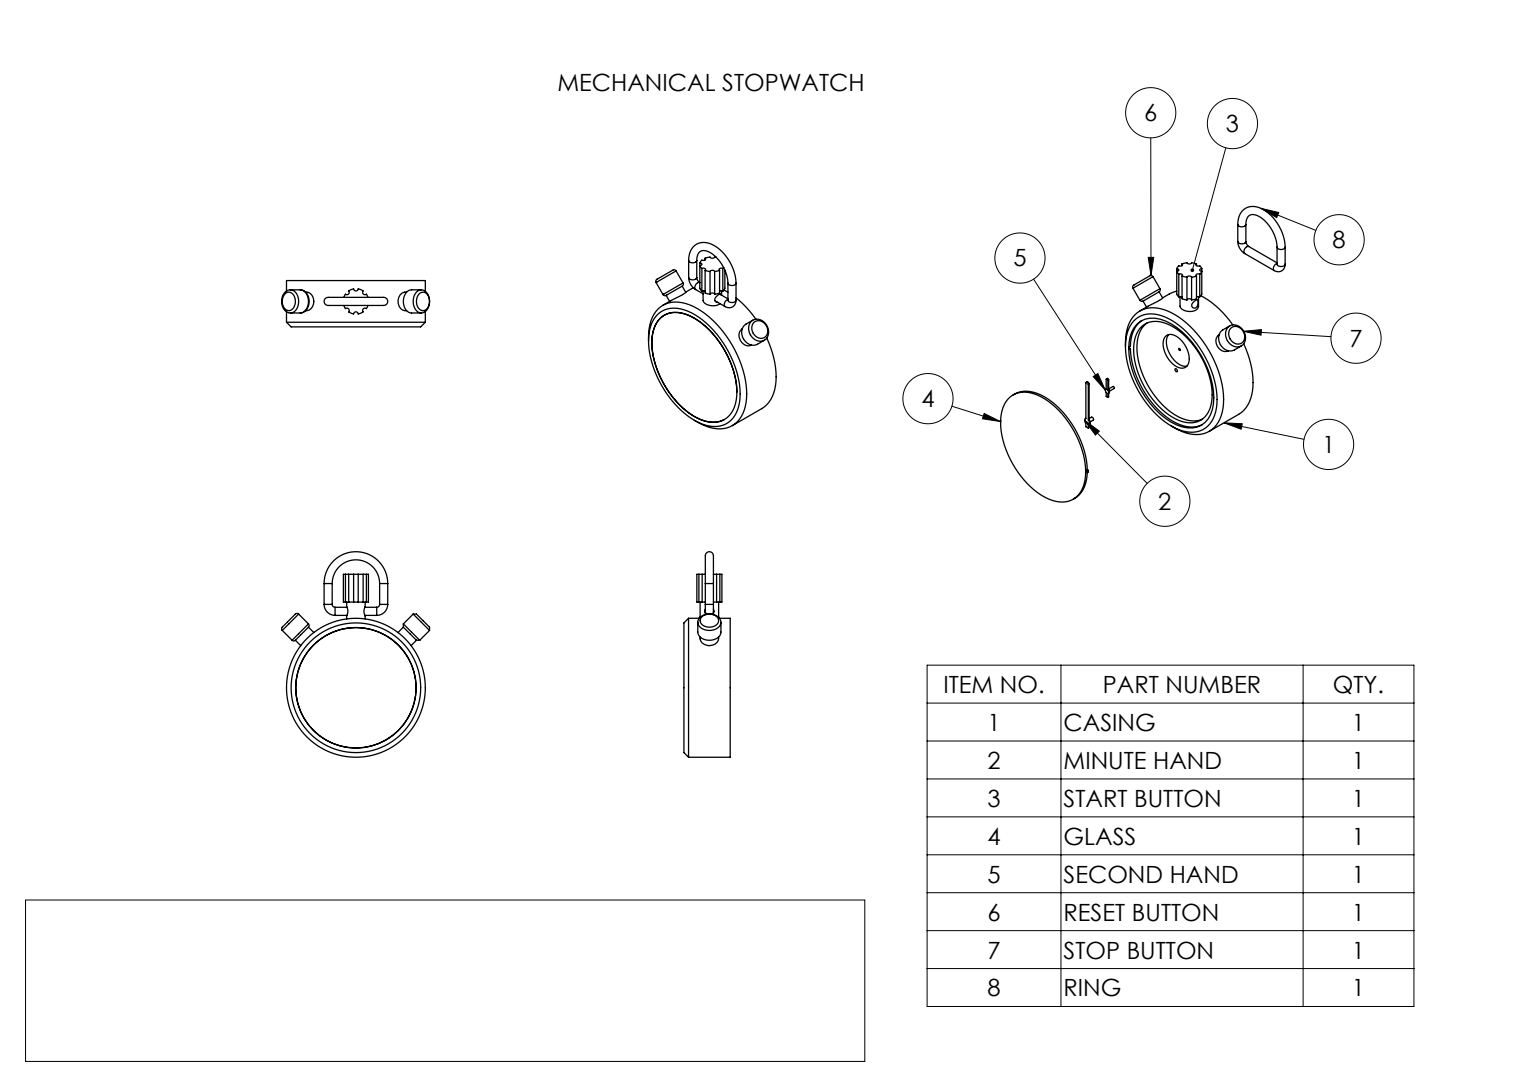
ISO-10303-21;
HEADER;
FILE_DESCRIPTION (('STEP AP214'),
    '1' );
FILE_NAME ('MAS-171',
    '2026-10-26T11:20:31',
    ( '' ),
    ( '' ),
    'SwSTEP 2.0',
    'SolidWorks 2026',
    '' );
FILE_SCHEMA (( 'AUTOMOTIVE_DESIGN' ));
ENDSEC;

DATA;
#1 = CARTESIAN_POINT ( 'NONE',  ( -0.7500000000000000000, 0.000000000000000000, 17.69999999999999929 ) ) ;
#2 = ORIENTED_EDGE ( 'NONE', *, *, #1110, .F. ) ;
#3 = ORIENTED_EDGE ( 'NONE', *, *, #2058, .T. ) ;
#4 = DIRECTION ( 'NONE',  ( 1.000000000000000000, 0.000000000000000000, 0.000000000000000000 ) ) ;
#5 = DIRECTION ( 'NONE',  ( 0.000000000000000000, 0.000000000000000000, 1.000000000000000000 ) ) ;
#6 = ORIENTED_EDGE ( 'NONE', *, *, #2251, .T. ) ;
#7 = ORIENTED_EDGE ( 'NONE', *, *, #1306, .T. ) ;
#8 = ORIENTED_EDGE ( 'NONE', *, *, #613, .T. ) ;
#9 = FACE_OUTER_BOUND ( 'NONE', #3478, .T. ) ;
#10 = MECHANICAL_DESIGN_GEOMETRIC_PRESENTATION_REPRESENTATION (  '', ( #2667 ), #1914 ) ;
#11 = CARTESIAN_POINT ( 'NONE',  ( 3.575465955037824273, 33.89312899261130951, 7.205771075917312807 ) ) ;
#12 = FILL_AREA_STYLE ('',( #728 ) ) ;
#13 = CARTESIAN_POINT ( 'NONE',  ( 3.900351855253538336, 31.20702153671021861, 9.895868398202676275 ) ) ;
#14 = APPLICATION_PROTOCOL_DEFINITION ( 'draft international standard', 'automotive_design', 1998, #590 ) ;
#15 = CIRCLE ( 'NONE', #3506, 24.00000000000000355 ) ;
#16 = AXIS2_PLACEMENT_3D ( 'NONE', #2193, #1531, #438 ) ;
#17 = CARTESIAN_POINT ( 'NONE',  ( 23.85222316637485562, 18.19536891688241198, 8.735393166554770161 ) ) ;
#18 = DIRECTION ( 'NONE',  ( -0.000000000000000000, -0.000000000000000000, -1.000000000000000000 ) ) ;
#19 = CARTESIAN_POINT ( 'NONE',  ( -0.5000000000000000000, -2.999999999999999556, 19.50000000000000000 ) ) ;
#20 = AXIS2_PLACEMENT_3D ( 'NONE', #4406, #1830, #790 ) ;
#21 = ORIENTED_EDGE ( 'NONE', *, *, #745, .T. ) ;
#22 = VERTEX_POINT ( 'NONE', #4223 ) ;
#23 = EDGE_CURVE ( 'NONE', #3682, #3477, #99, .T. ) ;
#24 = EDGE_CURVE ( 'NONE', #786, #1876, #1622, .T. ) ;
#25 = CARTESIAN_POINT ( 'NONE',  ( -3.889087296526001047, 37.00000000000000000, 5.110912703473974084 ) ) ;
#26 = DIRECTION ( 'NONE',  ( 0.000000000000000000, 0.000000000000000000, -1.000000000000000000 ) ) ;
#27 = VERTEX_POINT ( 'NONE', #607 ) ;
#28 = ORIENTED_EDGE ( 'NONE', *, *, #250, .F. ) ;
#29 = VERTEX_POINT ( 'NONE', #4130 ) ;
#30 = CARTESIAN_POINT ( 'NONE',  ( -8.999999999999998224, 36.00000000000000711, 0.000000000000000000 ) ) ;
#31 = CARTESIAN_POINT ( 'NONE',  ( -23.83674813237297130, 18.21571070649537916, 9.520895848189303123 ) ) ;
#32 =( LENGTH_UNIT ( ) NAMED_UNIT ( * ) SI_UNIT ( .MILLI., .METRE. ) );
#33 = CARTESIAN_POINT ( 'NONE',  ( -25.16843286583315376, -6.741346781237213648, 20.00001200000000168 ) ) ;
#34 = ORIENTED_EDGE ( 'NONE', *, *, #3765, .T. ) ;
#35 = APPLICATION_CONTEXT ( 'automotive_design' ) ;
#36 = AXIS2_PLACEMENT_3D ( 'NONE', #4466, #800, #1180 ) ;
#37 = CARTESIAN_POINT ( 'NONE',  ( 0.5000000000000001110, 6.123233995736767268E-17, 20.00000000000000000 ) ) ;
#38 = CARTESIAN_POINT ( 'NONE',  ( 0.000000000000000000, 10.00000000000000000, 13.00000000000000178 ) ) ;
#39 = CIRCLE ( 'NONE', #1106, 4.000000000000000000 ) ;
#40 = CARTESIAN_POINT ( 'NONE',  ( 18.61772044889877264, 23.52449179749628883, 6.992605352578564748 ) ) ;
#41 = CARTESIAN_POINT ( 'NONE',  ( -3.013274039476890653, 29.84885987243285399, 6.356496494711869616 ) ) ;
#42 = DIRECTION ( 'NONE',  ( 0.000000000000000000, 0.000000000000000000, 1.000000000000000000 ) ) ;
#43 = MECHANICAL_DESIGN_GEOMETRIC_PRESENTATION_REPRESENTATION (  '', ( #878 ), #2695 ) ;
#44 = ORIENTED_EDGE ( 'NONE', *, *, #3267, .F. ) ;
#45 = EDGE_CURVE ( 'NONE', #4134, #2111, #508, .T. ) ;
#46 = ORIENTED_EDGE ( 'NONE', *, *, #3772, .T. ) ;
#47 = CARTESIAN_POINT ( 'NONE',  ( -3.606497132222527213, 31.99144327829980838, 10.73188315364928691 ) ) ;
#48 = CIRCLE ( 'NONE', #1190, 1.749999999999999778 ) ;
#49 = DIRECTION ( 'NONE',  ( -0.000000000000000000, -0.000000000000000000, -1.000000000000000000 ) ) ;
#50 = EDGE_CURVE ( 'NONE', #1185, #1168, #2904, .T. ) ;
#51 = ORIENTED_EDGE ( 'NONE', *, *, #696, .F. ) ;
#52 = VERTEX_POINT ( 'NONE', #2322 ) ;
#53 = ORIENTED_EDGE ( 'NONE', *, *, #2142, .T. ) ;
#54 = EDGE_CURVE ( 'NONE', #3353, #742, #2591, .T. ) ;
#55 = CIRCLE ( 'NONE', #1867, 1.000000000000000000 ) ;
#56 = DIRECTION ( 'NONE',  ( 1.000000000000000000, 0.000000000000000000, -0.000000000000000000 ) ) ;
#57 = LINE ( 'NONE', #2588, #2669 ) ;
#58 = CARTESIAN_POINT ( 'NONE',  ( -0.5000000000000000000, 0.000000000000000000, 20.00000000000000000 ) ) ;
#59 = DIRECTION ( 'NONE',  ( 1.000000000000000000, 0.000000000000000000, 0.000000000000000000 ) ) ;
#60 = ORIENTED_EDGE ( 'NONE', *, *, #514, .T. ) ;
#61 = CARTESIAN_POINT ( 'NONE',  ( 3.120626071653185285, 37.00000000000000000, 4.471016347907789346 ) ) ;
#62 = DIRECTION ( 'NONE',  ( 0.000000000000000000, 0.000000000000000000, 1.000000000000000000 ) ) ;
#63 = CIRCLE ( 'NONE', #1740, 4.000000000000000000 ) ;
#64 = CARTESIAN_POINT ( 'NONE',  ( 21.58020450303990145, 20.84134157445924274, 5.025533726064748130 ) ) ;
#65 = DIRECTION ( 'NONE',  ( 0.000000000000000000, 1.000000000000000000, 0.000000000000000000 ) ) ;
#66 = TOROIDAL_SURFACE ( 'NONE', #1579, 12.00000000000000000, 1.749999999999999778 ) ;
#67 = FACE_OUTER_BOUND ( 'NONE', #3163, .T. ) ;
#68 = ADVANCED_FACE ( 'NONE', ( #4153 ), #1596, .T. ) ;
#69 = ORIENTED_EDGE ( 'NONE', *, *, #4531, .T. ) ;
#70 = ORIENTED_EDGE ( 'NONE', *, *, #687, .T. ) ;
#71 = EDGE_CURVE ( 'NONE', #1336, #2657, #200, .T. ) ;
#72 = AXIS2_PLACEMENT_3D ( 'NONE', #1710, #1001, #219 ) ;
#73 = CARTESIAN_POINT ( 'NONE',  ( -3.522877905629562711, 32.34829198493223146, 10.89542184998092367 ) ) ;
#74 = CARTESIAN_POINT ( 'NONE',  ( 3.469446951953614189E-15, 34.00000000000000000, 3.999999999999990674 ) ) ;
#75 = ORIENTED_EDGE ( 'NONE', *, *, #1897, .F. ) ;
#76 = EDGE_LOOP ( 'NONE', ( #1998, #356, #1571, #3856 ) ) ;
#77 = CIRCLE ( 'NONE', #3336, 1.749999999999999778 ) ;
#78 = ORIENTED_EDGE ( 'NONE', *, *, #3001, .F. ) ;
#79 = UNCERTAINTY_MEASURE_WITH_UNIT (LENGTH_MEASURE( 1.000000000000000082E-05 ), #706, 'distance_accuracy_value', 'NONE');
#80 = DIRECTION ( 'NONE',  ( 1.000000000000000000, -1.621111868633889227E-15, 0.000000000000000000 ) ) ;
#81 = CARTESIAN_POINT ( 'NONE',  ( -18.19536891688249014, 23.85222316637480233, 9.264542937126581279 ) ) ;
#82 = DIRECTION ( 'NONE',  ( 1.000000000000000000, 0.000000000000000000, 0.000000000000000000 ) ) ;
#83 = PLANE ( 'NONE',  #429 ) ;
#84 = EDGE_CURVE ( 'NONE', #2338, #1148, #4563, .T. ) ;
#85 = VERTEX_POINT ( 'NONE', #4577 ) ;
#86 = EDGE_CURVE ( 'NONE', #3119, #3855, #2573, .T. ) ;
#87 = LINE ( 'NONE', #2519, #444 ) ;
#88 = FACE_OUTER_BOUND ( 'NONE', #3234, .T. ) ;
#89 = CONTEXT_DEPENDENT_SHAPE_REPRESENTATION ( #4410, #2595 ) ;
#90 = AXIS2_PLACEMENT_3D ( 'NONE', #2223, #2270, #1567 ) ;
#91 = EDGE_CURVE ( 'NONE', #668, #4199, #3027, .T. ) ;
#92 = CARTESIAN_POINT ( 'NONE',  ( 23.23634976112698780, 18.97646788767667303, 6.355262957884884933 ) ) ;
#93 = PLANE ( 'NONE',  #36 ) ;
#94 = LINE ( 'NONE', #3342, #4161 ) ;
#95 = ORIENTED_EDGE ( 'NONE', *, *, #3675, .F. ) ;
#96 = ORIENTED_EDGE ( 'NONE', *, *, #3914, .F. ) ;
#97 = CARTESIAN_POINT ( 'NONE',  ( 0.000000000000000000, 0.000000000000000000, 17.69999999999999929 ) ) ;
#98 = DIRECTION ( 'NONE',  ( 0.000000000000000000, 0.000000000000000000, 1.000000000000000000 ) ) ;
#99 = CIRCLE ( 'NONE', #4660, 24.00000000000000355 ) ;
#100 = CIRCLE ( 'NONE', #1688, 1.749999999999999778 ) ;
#101 = CYLINDRICAL_SURFACE ( 'NONE', #1304, 4.000000000000000000 ) ;
#102 = VERTEX_POINT ( 'NONE', #652 ) ;
#103 = EDGE_LOOP ( 'NONE', ( #598, #2944, #3052, #880 ) ) ;
#104 = ORIENTED_EDGE ( 'NONE', *, *, #1011, .F. ) ;
#105 = EDGE_LOOP ( 'NONE', ( #1327, #855, #1076, #4619 ) ) ;
#106 = CARTESIAN_POINT ( 'NONE',  ( -3.889087296526001047, 37.00000000000000000, 5.110912703473974084 ) ) ;
#107 = CARTESIAN_POINT ( 'NONE',  ( -23.85222316637485207, 18.19536891688241553, 9.261144538644668245 ) ) ;
#108 = CARTESIAN_POINT ( 'NONE',  ( 27.09999999999999787, -0.5999999999999998668, 19.59999999999999787 ) ) ;
#109 = ORIENTED_EDGE ( 'NONE', *, *, #4683, .T. ) ;
#110 = CARTESIAN_POINT ( 'NONE',  ( 27.09999999999999787, -0.5999999999999998668, 19.00000000000000000 ) ) ;
#111 = CARTESIAN_POINT ( 'NONE',  ( 26.00000000000000355, 3.184081677783117796E-15, 19.59999999999999787 ) ) ;
#112 = ADVANCED_FACE ( 'NONE', ( #3592 ), #4601, .T. ) ;
#113 = ADVANCED_FACE ( 'NONE', ( #4266 ), #1343, .T. ) ;
#114 = CARTESIAN_POINT ( 'NONE',  ( 2.255140518769849223E-14, 37.00000000000000000, 4.499999999999992895 ) ) ;
#115 = CYLINDRICAL_SURFACE ( 'NONE', #1174, 24.00000000000000355 ) ;
#116 = CARTESIAN_POINT ( 'NONE',  ( -4.000043395258027878, 35.00008679053002680, 9.131973577465634762 ) ) ;
#117 = ORIENTED_EDGE ( 'NONE', *, *, #24, .F. ) ;
#118 = VECTOR ( 'NONE', #868, 1000.000000000000000 ) ;
#119 = DIRECTION ( 'NONE',  ( 0.000000000000000000, 0.000000000000000000, 1.000000000000000000 ) ) ;
#120 = CARTESIAN_POINT ( 'NONE',  ( 3.469446951953614189E-15, 37.00000000000000000, 8.999999999999992895 ) ) ;
#121 =( NAMED_UNIT ( * ) PLANE_ANGLE_UNIT ( ) SI_UNIT ( $, .RADIAN. ) );
#122 = AXIS2_PLACEMENT_3D ( 'NONE', #3838, #2369, #3476 ) ;
#123 = DIRECTION ( 'NONE',  ( -0.000000000000000000, -1.000000000000000000, -0.000000000000000000 ) ) ;
#124 = ORIENTED_EDGE ( 'NONE', *, *, #3765, .F. ) ;
#125 = ORIENTED_EDGE ( 'NONE', *, *, #1308, .T. ) ;
#126 = EDGE_LOOP ( 'NONE', ( #4196, #3326, #979, #96 ) ) ;
#127 = VERTEX_POINT ( 'NONE', #2121 ) ;
#128 = CARTESIAN_POINT ( 'NONE',  ( -0.5000000000000000000, -2.999999999999999556, 20.00000000000000000 ) ) ;
#129 =( GEOMETRIC_REPRESENTATION_CONTEXT ( 3 ) GLOBAL_UNCERTAINTY_ASSIGNED_CONTEXT ( ( #2638 ) ) GLOBAL_UNIT_ASSIGNED_CONTEXT ( ( #3790, #2760, #4527 ) ) REPRESENTATION_CONTEXT ( 'NONE', 'WORKASPACE' ) );
#130 = DIRECTION ( 'NONE',  ( 0.000000000000000000, 0.000000000000000000, 1.000000000000000000 ) ) ;
#131 = VECTOR ( 'NONE', #4325, 1000.000000000000000 ) ;
#132 = EDGE_CURVE ( 'NONE', #2734, #2850, #1760, .T. ) ;
#133 = DIRECTION ( 'NONE',  ( 0.000000000000000000, 0.000000000000000000, 1.000000000000000000 ) ) ;
#134 = ORIENTED_EDGE ( 'NONE', *, *, #2569, .F. ) ;
#135 = PRODUCT_DEFINITION_FORMATION_WITH_SPECIFIED_SOURCE ( 'ANY', '', #1681, .NOT_KNOWN. ) ;
#136 = AXIS2_PLACEMENT_3D ( 'NONE', #3423, #167, #2705 ) ;
#137 = DIRECTION ( 'NONE',  ( 0.000000000000000000, 0.000000000000000000, 1.000000000000000000 ) ) ;
#138 = DIRECTION ( 'NONE',  ( 0.000000000000000000, -0.000000000000000000, -1.000000000000000000 ) ) ;
#139 = CARTESIAN_POINT ( 'NONE',  ( 2.255140518769849223E-14, 37.00000000000000000, 3.499999999999992895 ) ) ;
#140 = DIRECTION ( 'NONE',  ( 0.000000000000000000, 0.000000000000000000, 1.000000000000000000 ) ) ;
#141 = CARTESIAN_POINT ( 'NONE',  ( -5.409090909090905619, 33.00000000000000000, 6.999999999999991118 ) ) ;
#142 = EDGE_CURVE ( 'NONE', #3182, #1602, #2491, .T. ) ;
#143 = DIRECTION ( 'NONE',  ( 1.000000000000000000, 0.000000000000000000, 0.000000000000000000 ) ) ;
#144 = AXIS2_PLACEMENT_3D ( 'NONE', #3788, #1981, #1244 ) ;
#145 = CARTESIAN_POINT ( 'NONE',  ( 3.809567799457752368, 34.58652683892340463, 10.22463024623739081 ) ) ;
#146 = CARTESIAN_POINT ( 'NONE',  ( 0.000000000000000000, 0.000000000000000000, 0.000000000000000000 ) ) ;
#147 = CARTESIAN_POINT ( 'NONE',  ( 0.000000000000000000, 0.000000000000000000, 20.00000000000000000 ) ) ;
#148 = ORIENTED_EDGE ( 'NONE', *, *, #3909, .T. ) ;
#149 = ORIENTED_EDGE ( 'NONE', *, *, #4614, .F. ) ;
#150 = ORIENTED_EDGE ( 'NONE', *, *, #4580, .T. ) ;
#151 = ORIENTED_EDGE ( 'NONE', *, *, #3914, .T. ) ;
#152 = CARTESIAN_POINT ( 'NONE',  ( -25.99307600111999150, -0.5999999999999996447, 19.00000000000000000 ) ) ;
#153 = UNCERTAINTY_MEASURE_WITH_UNIT (LENGTH_MEASURE( 1.000000000000000082E-05 ), #374, 'distance_accuracy_value', 'NONE');
#154 = SURFACE_STYLE_FILL_AREA ( #887 ) ;
#155 = SURFACE_SIDE_STYLE ('',( #1297 ) ) ;
#156 = DIRECTION ( 'NONE',  ( 0.000000000000000000, 0.000000000000000000, 1.000000000000000000 ) ) ;
#157 = CARTESIAN_POINT ( 'NONE',  ( -27.10000000000000497, -0.5999999999999998668, 19.00000000000000000 ) ) ;
#158 = DIRECTION ( 'NONE',  ( -0.000000000000000000, -1.000000000000000000, -0.000000000000000000 ) ) ;
#159 = CARTESIAN_POINT ( 'NONE',  ( 3.120626071653123113, 37.00000000000000000, 13.52898365209223996 ) ) ;
#160 = ORIENTED_EDGE ( 'NONE', *, *, #4437, .T. ) ;
#161 = VECTOR ( 'NONE', #2341, 1000.000000000000000 ) ;
#162 = CARTESIAN_POINT ( 'NONE',  ( -3.974466138550253103, 29.73560671006806899, 8.477544402765669673 ) ) ;
#163 = DIRECTION ( 'NONE',  ( -0.000000000000000000, -1.000000000000000000, 0.000000000000000000 ) ) ;
#164 = PLANE ( 'NONE',  #630 ) ;
#165 = CARTESIAN_POINT ( 'NONE',  ( 3.967498225428659264, 34.93431228236265440, 8.474567154859101947 ) ) ;
#166 = CARTESIAN_POINT ( 'NONE',  ( 0.000000000000000000, 0.000000000000000000, 0.000000000000000000 ) ) ;
#167 = DIRECTION ( 'NONE',  ( 0.000000000000000000, -0.000000000000000000, 1.000000000000000000 ) ) ;
#168 = ORIENTED_EDGE ( 'NONE', *, *, #2422, .T. ) ;
#169 = EDGE_LOOP ( 'NONE', ( #4072, #812, #3404, #1028 ) ) ;
#170 = EDGE_LOOP ( 'NONE', ( #191, #1020, #400, #4142, #3752, #2488, #1167, #3281, #3139 ) ) ;
#171 = EDGE_CURVE ( 'NONE', #2679, #1375, #2788, .T. ) ;
#172 = EDGE_LOOP ( 'NONE', ( #4370, #2757, #3708, #3979 ) ) ;
#173 = CIRCLE ( 'NONE', #776, 5.000000000000000888 ) ;
#174 = PLANE ( 'NONE',  #3718 ) ;
#175 = CARTESIAN_POINT ( 'NONE',  ( -1.734723475976807094E-15, 45.00000000000000000, 0.000000000000000000 ) ) ;
#176 = CIRCLE ( 'NONE', #3436, 4.000000000000000000 ) ;
#177 = VERTEX_POINT ( 'NONE', #3882 ) ;
#178 = LINE ( 'NONE', #2303, #3205 ) ;
#179 = CARTESIAN_POINT ( 'NONE',  ( 0.000000000000000000, 10.00000000000000000, 15.00000000000000178 ) ) ;
#180 = CARTESIAN_POINT ( 'NONE',  ( 8.000000000000000000, 10.00000000000000000, 15.00000000000000178 ) ) ;
#181 = VERTEX_POINT ( 'NONE', #3190 ) ;
#182 = FACE_OUTER_BOUND ( 'NONE', #1092, .T. ) ;
#183 = DIRECTION ( 'NONE',  ( -1.000000000000000000, 0.000000000000000000, 0.000000000000000000 ) ) ;
#184 = AXIS2_PLACEMENT_3D ( 'NONE', #568, #2063, #596 ) ;
#185 = CARTESIAN_POINT ( 'NONE',  ( -18.51903806033412891, 23.60202272616344743, 7.225073904196622543 ) ) ;
#186 = DIRECTION ( 'NONE',  ( 0.000000000000000000, 1.000000000000000000, 0.000000000000000000 ) ) ;
#187 = CARTESIAN_POINT ( 'NONE',  ( -24.67207871933484498, 8.377607117416790317, 20.00001200000000523 ) ) ;
#188 = ORIENTED_EDGE ( 'NONE', *, *, #4683, .F. ) ;
#189 = EDGE_CURVE ( 'NONE', #2680, #3477, #311, .T. ) ;
#190 = AXIS2_PLACEMENT_3D ( 'NONE', #1838, #4057, #3693 ) ;
#191 = ORIENTED_EDGE ( 'NONE', *, *, #3421, .T. ) ;
#192 = ORIENTED_EDGE ( 'NONE', *, *, #766, .F. ) ;
#193 = ADVANCED_FACE ( 'NONE', ( #334 ), #4702, .T. ) ;
#194 = ORIENTED_EDGE ( 'NONE', *, *, #171, .F. ) ;
#195 = CARTESIAN_POINT ( 'NONE',  ( 0.000000000000000000, 0.000000000000000000, 17.00000000000000000 ) ) ;
#196 = LINE ( 'NONE', #554, #4036 ) ;
#197 = VECTOR ( 'NONE', #3332, 1000.000000000000000 ) ;
#198 = EDGE_CURVE ( 'NONE', #954, #442, #3903, .T. ) ;
#199 = EDGE_CURVE ( 'NONE', #177, #2707, #3976, .T. ) ;
#200 = LINE ( 'NONE', #2032, #3955 ) ;
#201 = FACE_OUTER_BOUND ( 'NONE', #427, .T. ) ;
#202 = PLANE ( 'NONE',  #2959 ) ;
#203 = CARTESIAN_POINT ( 'NONE',  ( -3.889087296526055226, 49.00000000000000000, 12.88908729652595753 ) ) ;
#204 = EDGE_LOOP ( 'NONE', ( #2319, #1799, #3397, #669 ) ) ;
#205 = AXIS2_PLACEMENT_3D ( 'NONE', #2218, #4537, #1354 ) ;
#206 = PRODUCT ( 'glass', 'glass', '', ( #2572 ) ) ;
#207 = PRODUCT_DEFINITION_FORMATION_WITH_SPECIFIED_SOURCE ( 'ANY', '', #2064, .NOT_KNOWN. ) ;
#208 = CARTESIAN_POINT ( 'NONE',  ( 19.74742367678139132, 22.58509718322848769, 12.47015313278852844 ) ) ;
#209 = CARTESIAN_POINT ( 'NONE',  ( 1.000000000000000000, 0.000000000000000000, 20.00000000000000000 ) ) ;
#210 = CARTESIAN_POINT ( 'NONE',  ( -3.464101615137750390, 33.00000000000000000, 6.999999999999991118 ) ) ;
#211 = CARTESIAN_POINT ( 'NONE',  ( 3.469446951953614189E-15, 40.00000000000000000, 8.999999999999992895 ) ) ;
#212 = CARTESIAN_POINT ( 'NONE',  ( -13.02991752792604707, 22.56362157461192908, 20.00001199999999812 ) ) ;
#213 = VERTEX_POINT ( 'NONE', #2094 ) ;
#214 = ORIENTED_EDGE ( 'NONE', *, *, #364, .F. ) ;
#215 = EDGE_CURVE ( 'NONE', #3697, #378, #1086, .T. ) ;
#216 = ORIENTED_EDGE ( 'NONE', *, *, #4488, .T. ) ;
#217 = ORIENTED_EDGE ( 'NONE', *, *, #23, .F. ) ;
#218 = CIRCLE ( 'NONE', #2726, 1.250000000000002887 ) ;
#219 = DIRECTION ( 'NONE',  ( 1.000000000000000000, 0.000000000000000000, 0.000000000000000000 ) ) ;
#220 = DIRECTION ( 'NONE',  ( 0.000000000000000000, 0.000000000000000000, -1.000000000000000000 ) ) ;
#221 = DIRECTION ( 'NONE',  ( 0.000000000000000000, 0.000000000000000000, 1.000000000000000000 ) ) ;
#222 = AXIS2_PLACEMENT_3D ( 'NONE', #601, #2758, #3141 ) ;
#223 = ORIENTED_EDGE ( 'NONE', *, *, #3395, .T. ) ;
#224 = CARTESIAN_POINT ( 'NONE',  ( 0.000000000000000000, 10.00000000000000000, 13.00000000000000178 ) ) ;
#225 = AXIS2_PLACEMENT_3D ( 'NONE', #2885, #1132, #2148 ) ;
#226 = FACE_OUTER_BOUND ( 'NONE', #2584, .T. ) ;
#227 = EDGE_CURVE ( 'NONE', #883, #4468, #2767, .T. ) ;
#228 = ORIENTED_EDGE ( 'NONE', *, *, #457, .T. ) ;
#229 = EDGE_CURVE ( 'NONE', #3297, #3886, #3090, .T. ) ;
#230 = EDGE_CURVE ( 'NONE', #2552, #3925, #639, .T. ) ;
#231 = CARTESIAN_POINT ( 'NONE',  ( -3.889087296526001047, 34.17157287525380838, 5.110912703473974084 ) ) ;
#232 = CARTESIAN_POINT ( 'NONE',  ( -0.5000000000000000000, 0.000000000000000000, 19.50000000000000000 ) ) ;
#233 = VECTOR ( 'NONE', #4216, 1000.000000000000000 ) ;
#234 = CARTESIAN_POINT ( 'NONE',  ( 26.49999999999999645, -0.5000000000000000000, 19.50000000000000000 ) ) ;
#235 = CARTESIAN_POINT ( 'NONE',  ( 4.081770351527290718E-15, 41.00000000000000000, 13.99999999999999467 ) ) ;
#236 = DIRECTION ( 'NONE',  ( 0.000000000000000000, 0.000000000000000000, 1.000000000000000000 ) ) ;
#237 = ORIENTED_EDGE ( 'NONE', *, *, #1871, .T. ) ;
#238 = ORIENTED_EDGE ( 'NONE', *, *, #407, .F. ) ;
#239 = EDGE_LOOP ( 'NONE', ( #2558, #2162, #259, #4443, #4049, #3898, #2909, #3068 ) ) ;
#240 = FACE_OUTER_BOUND ( 'NONE', #4032, .T. ) ;
#241 = DIRECTION ( 'NONE',  ( 0.000000000000000000, 0.000000000000000000, 1.000000000000000000 ) ) ;
#242 = CARTESIAN_POINT ( 'NONE',  ( -3.403349963601461248, 25.83240171513484285, 20.00001200000000168 ) ) ;
#243 = CIRCLE ( 'NONE', #3040, 1.000000000000000000 ) ;
#244 = CARTESIAN_POINT ( 'NONE',  ( 8.999999999999996447, 34.74999999999999289, 2.143131898507865832E-16 ) ) ;
#245 = LINE ( 'NONE', #1716, #3549 ) ;
#246 = CARTESIAN_POINT ( 'NONE',  ( 3.469446951953614189E-15, 33.00000000000000000, 8.999999999999992895 ) ) ;
#247 = VECTOR ( 'NONE', #3763, 1000.000000000000000 ) ;
#248 = VECTOR ( 'NONE', #2476, 1000.000000000000000 ) ;
#249 = ORIENTED_EDGE ( 'NONE', *, *, #4128, .F. ) ;
#250 = EDGE_CURVE ( 'NONE', #1339, #1902, #257, .T. ) ;
#251 = CARTESIAN_POINT ( 'NONE',  ( 18.51766120599535981, 23.60309964903844104, 10.77116693461329078 ) ) ;
#252 = PLANE ( 'NONE',  #505 ) ;
#253 = EDGE_CURVE ( 'NONE', #1148, #1902, #1067, .T. ) ;
#254 = ADVANCED_FACE ( 'NONE', ( #2730 ), #1312, .F. ) ;
#255 = DIRECTION ( 'NONE',  ( 0.000000000000000000, 0.000000000000000000, 1.000000000000000000 ) ) ;
#256 = FACE_OUTER_BOUND ( 'NONE', #2832, .T. ) ;
#257 = LINE ( 'NONE', #3875, #233 ) ;
#258 = ORIENTED_EDGE ( 'NONE', *, *, #4554, .T. ) ;
#259 = ORIENTED_EDGE ( 'NONE', *, *, #1804, .T. ) ;
#260 = AXIS2_PLACEMENT_3D ( 'NONE', #4512, #2060, #1677 ) ;
#261 = DIRECTION ( 'NONE',  ( 0.000000000000000000, 0.000000000000000000, 1.000000000000000000 ) ) ;
#262 = FACE_OUTER_BOUND ( 'NONE', #1955, .T. ) ;
#263 =( LENGTH_UNIT ( ) NAMED_UNIT ( * ) SI_UNIT ( .MILLI., .METRE. ) );
#264 = AXIS2_PLACEMENT_3D ( 'NONE', #4299, #3243, #659 ) ;
#265 = SURFACE_SIDE_STYLE ('',( #3589 ) ) ;
#266 = CARTESIAN_POINT ( 'NONE',  ( 27.09999999999999787, -0.5999999999999998668, 19.59999999999999787 ) ) ;
#267 = ADVANCED_FACE ( 'NONE', ( #621 ), #905, .F. ) ;
#268 = AXIS2_PLACEMENT_3D ( 'NONE', #458, #2589, #3308 ) ;
#269 = DIRECTION ( 'NONE',  ( -0.000000000000000000, -1.000000000000000000, -0.000000000000000000 ) ) ;
#270 = DIRECTION ( 'NONE',  ( 0.000000000000000000, 0.000000000000000000, 1.000000000000000000 ) ) ;
#271 = CARTESIAN_POINT ( 'NONE',  ( 0.2611446086310952874, 29.99999999999999645, 12.99999999999999112 ) ) ;
#272 = ORIENTED_EDGE ( 'NONE', *, *, #761, .F. ) ;
#273 = DIRECTION ( 'NONE',  ( 0.000000000000000000, 1.000000000000000000, 0.000000000000000000 ) ) ;
#274 =( REPRESENTATION_RELATIONSHIP ('NONE','NONE', #2397, #4641 ) REPRESENTATION_RELATIONSHIP_WITH_TRANSFORMATION ( #1227 )SHAPE_REPRESENTATION_RELATIONSHIP( ) );
#275 = DIRECTION ( 'NONE',  ( 0.000000000000000000, 0.000000000000000000, 1.000000000000000000 ) ) ;
#276 = CARTESIAN_POINT ( 'NONE',  ( 0.7500000000000001110, 0.000000000000000000, 17.00000000000000000 ) ) ;
#277 = VECTOR ( 'NONE', #1465, 1000.000000000000000 ) ;
#278 = CARTESIAN_POINT ( 'NONE',  ( 17.67766952966372429, 17.67766952966365679, 8.999999999999992895 ) ) ;
#279 = LINE ( 'NONE', #643, #686 ) ;
#280 = FACE_OUTER_BOUND ( 'NONE', #719, .T. ) ;
#281 = EDGE_CURVE ( 'NONE', #1290, #3612, #2017, .T. ) ;
#282 = ORIENTED_EDGE ( 'NONE', *, *, #4614, .T. ) ;
#283 = EDGE_CURVE ( 'NONE', #741, #1146, #1292, .T. ) ;
#284 = ORIENTED_EDGE ( 'NONE', *, *, #1600, .T. ) ;
#285 = LINE ( 'NONE', #1756, #509 ) ;
#286 = CARTESIAN_POINT ( 'NONE',  ( 3.469446951953614189E-15, 49.00000000000000000, 8.999999999999992895 ) ) ;
#287 = SHAPE_REPRESENTATION_RELATIONSHIP ( 'NONE' , 'NONE' ,  #1408, #2500 ) ;
#288 = PRODUCT_DEFINITION_CONTEXT ( 'detailed design', #920, 'design' ) ;
#289 = VERTEX_POINT ( 'NONE', #3854 ) ;
#290 = DIRECTION ( 'NONE',  ( -1.000000000000000000, 0.000000000000000000, 0.000000000000000000 ) ) ;
#291 = AXIS2_PLACEMENT_3D ( 'NONE', #4539, #997, #2087 ) ;
#292 = CARTESIAN_POINT ( 'NONE',  ( -0.7500000000000001110, 20.00000000000000000, 18.19999999999999929 ) ) ;
#293 = CARTESIAN_POINT ( 'NONE',  ( -3.120626071653146649, 43.00000000000000000, 4.471016347907768029 ) ) ;
#294 = CIRCLE ( 'NONE', #1500, 1.000000000000000000 ) ;
#295 = CARTESIAN_POINT ( 'NONE',  ( 1.289767132401806071, 29.97323123820465440, 12.79530979536915858 ) ) ;
#296 = AXIS2_PLACEMENT_3D ( 'NONE', #2408, #3159, #4617 ) ;
#297 = PRESENTATION_LAYER_ASSIGNMENT (  '', '', ( #2330 ) ) ;
#298 = SURFACE_STYLE_FILL_AREA ( #2126 ) ;
#299 = CARTESIAN_POINT ( 'NONE',  ( 25.99307600111999150, -0.5999999999999996447, 19.00000000000000000 ) ) ;
#300 = CARTESIAN_POINT ( 'NONE',  ( 25.83240171513484285, -3.403349963601437267, 20.00001200000000168 ) ) ;
#301 = CARTESIAN_POINT ( 'NONE',  ( -22.58496929628987360, 19.74756467586668762, 5.529782636833617815 ) ) ;
#302 = CARTESIAN_POINT ( 'NONE',  ( 0.000000000000000000, 0.000000000000000000, 16.00000000000000000 ) ) ;
#303 = CARTESIAN_POINT ( 'NONE',  ( 9.000000000000003553, 36.00000000000000000, 2.143131898507868051E-16 ) ) ;
#304 = ORIENTED_EDGE ( 'NONE', *, *, #711, .T. ) ;
#305 = VERTEX_POINT ( 'NONE', #1266 ) ;
#306 = CARTESIAN_POINT ( 'NONE',  ( 5.500000000000003553, 34.17157287525380838, 8.999999999999992895 ) ) ;
#307 = VECTOR ( 'NONE', #4096, 1000.000000000000000 ) ;
#308 = CARTESIAN_POINT ( 'NONE',  ( 3.469446951953614189E-15, 34.00000000000000000, 8.999999999999992895 ) ) ;
#309 = EDGE_CURVE ( 'NONE', #2969, #127, #2118, .T. ) ;
#310 = VERTEX_POINT ( 'NONE', #3063 ) ;
#311 = LINE ( 'NONE', #4676, #943 ) ;
#312 = ADVANCED_FACE ( 'NONE', ( #2776 ), #4236, .F. ) ;
#313 = DIRECTION ( 'NONE',  ( 1.000000000000000000, 0.000000000000000000, 0.000000000000000000 ) ) ;
#314 = CARTESIAN_POINT ( 'NONE',  ( 3.469446951953614189E-15, 34.00000000000000000, 8.999999999999992895 ) ) ;
#315 = CARTESIAN_POINT ( 'NONE',  ( 1.037548646792561202, 29.98316644498967776, 12.87206112426449955 ) ) ;
#316 = DIRECTION ( 'NONE',  ( 0.000000000000000000, 0.000000000000000000, -1.000000000000000000 ) ) ;
#317 = PRODUCT_DEFINITION_SHAPE ( 'NONE', 'NONE',  #4714 ) ;
#318 = AXIS2_PLACEMENT_3D ( 'NONE', #3626, #2522, #799 ) ;
#319 = CARTESIAN_POINT ( 'NONE',  ( 3.993269581196953411, 31.01336414471273883, 8.733908321742495318 ) ) ;
#320 = PRODUCT_CONTEXT ( 'NONE', #3923, 'mechanical' ) ;
#321 = CARTESIAN_POINT ( 'NONE',  ( -26.00000000000000355, -1.592040838891558504E-15, 20.00000599999999906 ) ) ;
#322 = AXIS2_PLACEMENT_3D ( 'NONE', #4183, #3766, #484 ) ;
#323 = DIRECTION ( 'NONE',  ( -0.000000000000000000, -1.000000000000000000, -0.000000000000000000 ) ) ;
#324 = LINE ( 'NONE', #1796, #4294 ) ;
#325 = DIRECTION ( 'NONE',  ( 0.000000000000000000, 0.000000000000000000, 1.000000000000000000 ) ) ;
#326 = EDGE_LOOP ( 'NONE', ( #3897, #833, #3483, #60 ) ) ;
#327 = ORIENTED_EDGE ( 'NONE', *, *, #457, .F. ) ;
#328 = DIRECTION ( 'NONE',  ( 1.000000000000000000, -0.000000000000000000, 1.224646799147353207E-16 ) ) ;
#329 = SURFACE_SIDE_STYLE ('',( #2159 ) ) ;
#330 = DIRECTION ( 'NONE',  ( -1.000000000000000000, 0.000000000000000000, -0.000000000000000000 ) ) ;
#331 = PLANE ( 'NONE',  #3572 ) ;
#332 = ADVANCED_FACE ( 'NONE', ( #1356 ), #2431, .F. ) ;
#333 = ORIENTED_EDGE ( 'NONE', *, *, #4326, .T. ) ;
#334 = FACE_OUTER_BOUND ( 'NONE', #3811, .T. ) ;
#335 = APPLICATION_CONTEXT ( 'automotive_design' ) ;
#336 = DIRECTION ( 'NONE',  ( 0.7071067811865487940, -0.7071067811865463515, 0.000000000000000000 ) ) ;
#337 = AXIS2_PLACEMENT_3D ( 'NONE', #302, #2550, #4345 ) ;
#338 = CARTESIAN_POINT ( 'NONE',  ( 0.000000000000000000, 0.000000000000000000, 17.00000000000000000 ) ) ;
#339 = CARTESIAN_POINT ( 'NONE',  ( 2.445228802079471908, 29.90098466201939331, 5.823513562339502236 ) ) ;
#340 = AXIS2_PLACEMENT_3D ( 'NONE', #4186, #2765, #968 ) ;
#341 = DIRECTION ( 'NONE',  ( 1.000000000000000000, -0.000000000000000000, -0.000000000000000000 ) ) ;
#342 = VECTOR ( 'NONE', #432, 1000.000000000000000 ) ;
#343 = CARTESIAN_POINT ( 'NONE',  ( 22.99946665860936079, 19.26288713789788076, 12.01444203287436174 ) ) ;
#344 = SHAPE_DEFINITION_REPRESENTATION ( #546, #4641 ) ;
#345 = MECHANICAL_DESIGN_GEOMETRIC_PRESENTATION_REPRESENTATION (  '', ( #2384 ), #129 ) ;
#346 = CARTESIAN_POINT ( 'NONE',  ( 3.469446951953614189E-15, 40.00000000000000000, 12.99999999999999467 ) ) ;
#347 = DIRECTION ( 'NONE',  ( -1.000000000000000000, -0.000000000000000000, -0.000000000000000000 ) ) ;
#348 = CARTESIAN_POINT ( 'NONE',  ( -0.5000000000000000000, -0.8660254037844387076, 19.50000000000000000 ) ) ;
#349 = CIRCLE ( 'NONE', #1112, 5.000000000000002665 ) ;
#350 = ORIENTED_EDGE ( 'NONE', *, *, #987, .F. ) ;
#351 = EDGE_LOOP ( 'NONE', ( #3080, #1048, #1376, #4284 ) ) ;
#352 = CARTESIAN_POINT ( 'NONE',  ( 3.469446951953614189E-15, 41.00000000000000000, 8.999999999999992895 ) ) ;
#353 = DIRECTION ( 'NONE',  ( 0.000000000000000000, 0.000000000000000000, 1.000000000000000000 ) ) ;
#354 = ORIENTED_EDGE ( 'NONE', *, *, #189, .T. ) ;
#355 = ORIENTED_EDGE ( 'NONE', *, *, #1156, .F. ) ;
#356 = ORIENTED_EDGE ( 'NONE', *, *, #4437, .F. ) ;
#357 = DIRECTION ( 'NONE',  ( -0.000000000000000000, -0.000000000000000000, -1.000000000000000000 ) ) ;
#358 = CARTESIAN_POINT ( 'NONE',  ( 3.999885695961631793, 34.99977139185988051, 9.266511461428612151 ) ) ;
#359 = CARTESIAN_POINT ( 'NONE',  ( -5.409090909090905619, 43.00000000000000000, 9.995859195463930646 ) ) ;
#360 = VECTOR ( 'NONE', #3662, 1000.000000000000000 ) ;
#361 = CARTESIAN_POINT ( 'NONE',  ( 3.464101615137758383, 32.86534535152231484, 6.999999999999992006 ) ) ;
#362 = APPLICATION_PROTOCOL_DEFINITION ( 'draft international standard', 'automotive_design', 1998, #35 ) ;
#363 = EDGE_CURVE ( 'NONE', #3116, #786, #4257, .T. ) ;
#364 = EDGE_CURVE ( 'NONE', #2850, #4511, #2465, .T. ) ;
#365 = CIRCLE ( 'NONE', #72, 0.5000000000000001110 ) ;
#366 = CARTESIAN_POINT ( 'NONE',  ( 4.528983652092195555, 37.00000000000000000, 12.12062607165318973 ) ) ;
#367 = AXIS2_PLACEMENT_3D ( 'NONE', #1611, #4592, #2382 ) ;
#368 = AXIS2_PLACEMENT_3D ( 'NONE', #485, #3386, #138 ) ;
#369 = DIRECTION ( 'NONE',  ( -1.000000000000000000, 0.000000000000000000, 0.000000000000000000 ) ) ;
#370 = FACE_OUTER_BOUND ( 'NONE', #716, .T. ) ;
#371 = ORIENTED_EDGE ( 'NONE', *, *, #2152, .T. ) ;
#372 = EDGE_LOOP ( 'NONE', ( #1130, #2275, #3372, #4073 ) ) ;
#373 = DIRECTION ( 'NONE',  ( 0.000000000000000000, 0.000000000000000000, 1.000000000000000000 ) ) ;
#374 =( LENGTH_UNIT ( ) NAMED_UNIT ( * ) SI_UNIT ( .MILLI., .METRE. ) );
#375 = DIRECTION ( 'NONE',  ( 0.000000000000000000, 0.000000000000000000, 1.000000000000000000 ) ) ;
#376 = ORIENTED_EDGE ( 'NONE', *, *, #4634, .F. ) ;
#377 = VERTEX_POINT ( 'NONE', #3443 ) ;
#378 = VERTEX_POINT ( 'NONE', #2133 ) ;
#379 = LINE ( 'NONE', #4051, #4102 ) ;
#380 = AXIS2_PLACEMENT_3D ( 'NONE', #2484, #3587, #1024 ) ;
#381 = FACE_OUTER_BOUND ( 'NONE', #4174, .T. ) ;
#382 = FACE_OUTER_BOUND ( 'NONE', #909, .T. ) ;
#383 = EDGE_LOOP ( 'NONE', ( #2433, #2317, #125, #4259 ) ) ;
#384 = CARTESIAN_POINT ( 'NONE',  ( 0.5000000000000000000, 0.000000000000000000, 19.50000000000000000 ) ) ;
#385 = CARTESIAN_POINT ( 'NONE',  ( 3.469446951953614189E-15, 33.00000000000000000, 8.999999999999992895 ) ) ;
#386 = ADVANCED_FACE ( 'NONE', ( #370 ), #2455, .F. ) ;
#387 = AXIS2_PLACEMENT_3D ( 'NONE', #4457, #1221, #2661 ) ;
#388 = CARTESIAN_POINT ( 'NONE',  ( 23.60202272616350783, 18.51903806033405075, 7.225073904196623431 ) ) ;
#389 = CARTESIAN_POINT ( 'NONE',  ( 26.00000000000000711, 3.184081677783118980E-15, 20.00000000000000000 ) ) ;
#390 = EDGE_CURVE ( 'NONE', #3925, #1876, #667, .T. ) ;
#391 = CARTESIAN_POINT ( 'NONE',  ( -3.967441838779837582, 34.93419588968778555, 9.525690396061339271 ) ) ;
#392 = ADVANCED_FACE ( 'NONE', ( #280 ), #3556, .F. ) ;
#393 = VECTOR ( 'NONE', #632, 1000.000000000000000 ) ;
#394 = ORIENTED_EDGE ( 'NONE', *, *, #1600, .F. ) ;
#395 = EDGE_LOOP ( 'NONE', ( #4328, #2140, #4671, #3538 ) ) ;
#396 = DIRECTION ( 'NONE',  ( 1.000000000000000000, 0.000000000000000000, -0.000000000000000000 ) ) ;
#397 =( NAMED_UNIT ( * ) SI_UNIT ( $, .STERADIAN. ) SOLID_ANGLE_UNIT ( ) );
#398 = FACE_OUTER_BOUND ( 'NONE', #695, .T. ) ;
#399 = ORIENTED_EDGE ( 'NONE', *, *, #2054, .T. ) ;
#400 = ORIENTED_EDGE ( 'NONE', *, *, #1846, .F. ) ;
#401 = ORIENTED_EDGE ( 'NONE', *, *, #3956, .F. ) ;
#402 = CARTESIAN_POINT ( 'NONE',  ( 0.7500000000000000000, -2.999999999999999556, 17.69999999999999929 ) ) ;
#403 = DIRECTION ( 'NONE',  ( -0.000000000000000000, 1.000000000000000000, -0.000000000000000000 ) ) ;
#404 = SHAPE_REPRESENTATION ( 'second hand', ( #2928 ), #3465 ) ;
#405 = FACE_OUTER_BOUND ( 'NONE', #3345, .T. ) ;
#406 = DIRECTION ( 'NONE',  ( -0.000000000000000000, -0.000000000000000000, 1.000000000000000000 ) ) ;
#407 = EDGE_CURVE ( 'NONE', #4099, #956, #3629, .T. ) ;
#408 = ORIENTED_EDGE ( 'NONE', *, *, #542, .F. ) ;
#409 = AXIS2_PLACEMENT_3D ( 'NONE', #952, #3826, #4194 ) ;
#410 = EDGE_CURVE ( 'NONE', #1443, #3515, #349, .T. ) ;
#411 = CARTESIAN_POINT ( 'NONE',  ( 3.522982843720159796, 32.34803768106982602, 10.89519766348715102 ) ) ;
#412 = CIRCLE ( 'NONE', #3674, 1.000000000000000000 ) ;
#413 = VECTOR ( 'NONE', #4600, 1000.000000000000000 ) ;
#414 = CARTESIAN_POINT ( 'NONE',  ( 22.43029000766442493, 19.92335677698576291, 5.404794703904384434 ) ) ;
#415 = CARTESIAN_POINT ( 'NONE',  ( -3.889087296526001047, 49.00000000000000000, 6.110912703473974084 ) ) ;
#416 = FACE_OUTER_BOUND ( 'NONE', #1243, .T. ) ;
#417 = EDGE_LOOP ( 'NONE', ( #3095, #2362, #3318, #3383, #3652 ) ) ;
#418 = VERTEX_POINT ( 'NONE', #4346 ) ;
#419 = CARTESIAN_POINT ( 'NONE',  ( 0.7500000000000001110, 1.299038105676658450, 17.69999999999999929 ) ) ;
#420 = PRESENTATION_LAYER_ASSIGNMENT (  '', '', ( #2384 ) ) ;
#421 = AXIS2_PLACEMENT_3D ( 'NONE', #2479, #3250, #1065 ) ;
#422 = APPLICATION_CONTEXT ( 'automotive_design' ) ;
#423 = CYLINDRICAL_SURFACE ( 'NONE', #4197, 1.000000000000000000 ) ;
#424 = EDGE_LOOP ( 'NONE', ( #1754, #498 ) ) ;
#425 = ADVANCED_FACE ( 'NONE', ( #2551 ), #3201, .T. ) ;
#426 = ORIENTED_EDGE ( 'NONE', *, *, #1762, .F. ) ;
#427 = EDGE_LOOP ( 'NONE', ( #1515, #2000, #282, #1851 ) ) ;
#428 = AXIS2_PLACEMENT_3D ( 'NONE', #146, #1975, #877 ) ;
#429 = AXIS2_PLACEMENT_3D ( 'NONE', #1371, #641, #2955 ) ;
#430 = DIRECTION ( 'NONE',  ( -1.000000000000000000, 0.000000000000000000, 0.000000000000000000 ) ) ;
#431 = CARTESIAN_POINT ( 'NONE',  ( -23.77376218378628181, 18.29783893517727478, 10.03754308049874311 ) ) ;
#432 = DIRECTION ( 'NONE',  ( 0.000000000000000000, -1.000000000000000000, 0.000000000000000000 ) ) ;
#433 = CARTESIAN_POINT ( 'NONE',  ( 26.00000000000000355, 1.592040838891558898E-15, 20.00000599999999906 ) ) ;
#434 = ORIENTED_EDGE ( 'NONE', *, *, #4128, .T. ) ;
#435 = DIRECTION ( 'NONE',  ( -1.000000000000000000, 0.000000000000000000, -0.000000000000000000 ) ) ;
#436 = CYLINDRICAL_SURFACE ( 'NONE', #571, 3.999999999999998224 ) ;
#437 = AXIS2_PLACEMENT_3D ( 'NONE', #3171, #2146, #3524 ) ;
#438 = DIRECTION ( 'NONE',  ( 0.000000000000000000, 0.000000000000000000, 1.000000000000000000 ) ) ;
#439 = CARTESIAN_POINT ( 'NONE',  ( -5.499999999999996447, 34.17157287525380838, 8.999999999999992895 ) ) ;
#440 = VECTOR ( 'NONE', #3448, 1000.000000000000000 ) ;
#441 = CARTESIAN_POINT ( 'NONE',  ( -3.672134815396410179, 34.23001392835894308, 10.59780778022629377 ) ) ;
#442 = VERTEX_POINT ( 'NONE', #348 ) ;
#443 = ORIENTED_EDGE ( 'NONE', *, *, #2740, .F. ) ;
#444 = VECTOR ( 'NONE', #4378, 1000.000000000000000 ) ;
#445 = CARTESIAN_POINT ( 'NONE',  ( -3.501495480098614443, 32.47366590808272235, 10.93402018205975601 ) ) ;
#446 = CARTESIAN_POINT ( 'NONE',  ( 3.469446951953614189E-15, 49.00000000000000000, 8.999999999999992895 ) ) ;
#447 =( LENGTH_UNIT ( ) NAMED_UNIT ( * ) SI_UNIT ( .MILLI., .METRE. ) );
#448 = CARTESIAN_POINT ( 'NONE',  ( 3.469446951953614189E-15, 49.00000000000000000, 8.999999999999992895 ) ) ;
#449 = ORIENTED_EDGE ( 'NONE', *, *, #3217, .T. ) ;
#450 = ORIENTED_EDGE ( 'NONE', *, *, #688, .F. ) ;
#451 = AXIS2_PLACEMENT_3D ( 'NONE', #3078, #2717, #4317 ) ;
#452 = ORIENTED_EDGE ( 'NONE', *, *, #2236, .F. ) ;
#453 = UNCERTAINTY_MEASURE_WITH_UNIT (LENGTH_MEASURE( 1.000000000000000082E-05 ), #1801, 'distance_accuracy_value', 'NONE');
#454 = CARTESIAN_POINT ( 'NONE',  ( -0.5000000000000001110, 0.000000000000000000, 16.00000000000000000 ) ) ;
#455 = CARTESIAN_POINT ( 'NONE',  ( 8.999999999999980460, 32.99999999999999289, 0.000000000000000000 ) ) ;
#456 = VECTOR ( 'NONE', #3934, 1000.000000000000000 ) ;
#457 = EDGE_CURVE ( 'NONE', #2385, #2339, #3083, .T. ) ;
#458 = CARTESIAN_POINT ( 'NONE',  ( 0.000000000000000000, 10.00000000000000000, 15.00000000000000178 ) ) ;
#459 = EDGE_CURVE ( 'NONE', #2022, #1315, #48, .T. ) ;
#460 = VERTEX_POINT ( 'NONE', #3272 ) ;
#461 = CARTESIAN_POINT ( 'NONE',  ( -0.5000000000000000000, 6.000000000000000000, 19.50000000000000000 ) ) ;
#462 = CARTESIAN_POINT ( 'NONE',  ( -27.10000000000000497, -0.5999999999999998668, 19.59999999999999787 ) ) ;
#463 = VECTOR ( 'NONE', #1245, 1000.000000000000000 ) ;
#464 = CARTESIAN_POINT ( 'NONE',  ( 0.5000000000000000000, -2.999999999999999556, 19.50000000000000000 ) ) ;
#465 = CARTESIAN_POINT ( 'NONE',  ( 0.000000000000000000, 0.000000000000000000, 17.99999999999998579 ) ) ;
#466 = DIRECTION ( 'NONE',  ( 1.000000000000000000, 0.000000000000000000, -0.000000000000000000 ) ) ;
#467 = CIRCLE ( 'NONE', #1081, 1.000000000000000000 ) ;
#468 = VERTEX_POINT ( 'NONE', #4017 ) ;
#469 = EDGE_CURVE ( 'NONE', #29, #4376, #2892, .T. ) ;
#470 = CARTESIAN_POINT ( 'NONE',  ( -17.67766952966371719, 17.67766952966366389, 8.999999999999992895 ) ) ;
#471 = CARTESIAN_POINT ( 'NONE',  ( -27.10000000000000497, -0.5999999999999998668, 19.00000000000000000 ) ) ;
#472 = VECTOR ( 'NONE', #1598, 1000.000000000000000 ) ;
#473 = SURFACE_STYLE_FILL_AREA ( #1539 ) ;
#474 = FACE_OUTER_BOUND ( 'NONE', #326, .T. ) ;
#475 = ORIENTED_EDGE ( 'NONE', *, *, #410, .F. ) ;
#476 = ORIENTED_EDGE ( 'NONE', *, *, #1700, .F. ) ;
#477 = VERTEX_POINT ( 'NONE', #2505 ) ;
#478 = ORIENTED_EDGE ( 'NONE', *, *, #3950, .F. ) ;
#479 = DIRECTION ( 'NONE',  ( 0.000000000000000000, 1.000000000000000000, 0.000000000000000000 ) ) ;
#480 = CARTESIAN_POINT ( 'NONE',  ( -18.61790092284054410, 23.52435923723752609, 11.00811882721853152 ) ) ;
#481 = UNCERTAINTY_MEASURE_WITH_UNIT (LENGTH_MEASURE( 1.000000000000000082E-05 ), #3442, 'distance_accuracy_value', 'NONE');
#482 = LINE ( 'NONE', #3407, #3156 ) ;
#483 = ORIENTED_EDGE ( 'NONE', *, *, #4706, .T. ) ;
#484 = DIRECTION ( 'NONE',  ( 1.000000000000000000, 0.000000000000000000, 0.000000000000000000 ) ) ;
#485 = CARTESIAN_POINT ( 'NONE',  ( -27.10000000000000497, 0.6000000000000000888, 19.59999999999999787 ) ) ;
#486 = CARTESIAN_POINT ( 'NONE',  ( 3.601048973789312324, 31.98899025511026650, 10.74504312029988284 ) ) ;
#487 = PRODUCT_DEFINITION ( 'UNKNOWN', '', #1349, #2416 ) ;
#488 = CIRCLE ( 'NONE', #2609, 26.00000000000000711 ) ;
#489 = CIRCLE ( 'NONE', #2768, 1.750000000000001554 ) ;
#490 = CARTESIAN_POINT ( 'NONE',  ( -1.774938052278379752, 29.94842879300231075, 5.405792698933810314 ) ) ;
#491 = FACE_OUTER_BOUND ( 'NONE', #3092, .T. ) ;
#492 = ORIENTED_EDGE ( 'NONE', *, *, #132, .T. ) ;
#493 = CYLINDRICAL_SURFACE ( 'NONE', #995, 1.749999999999999778 ) ;
#494 = CARTESIAN_POINT ( 'NONE',  ( 3.971780439164239063, 34.94497680528392891, 9.533653685786569909 ) ) ;
#495 = DIRECTION ( 'NONE',  ( 1.000000000000000000, 0.000000000000000000, 0.000000000000000000 ) ) ;
#496 = PRESENTATION_LAYER_ASSIGNMENT (  '', '', ( #3462 ) ) ;
#497 = DIRECTION ( 'NONE',  ( 0.000000000000000000, 0.000000000000000000, 1.000000000000000000 ) ) ;
#498 = ORIENTED_EDGE ( 'NONE', *, *, #3330, .T. ) ;
#499 = VERTEX_POINT ( 'NONE', #19 ) ;
#500 = ORIENTED_EDGE ( 'NONE', *, *, #1073, .F. ) ;
#501 = ORIENTED_EDGE ( 'NONE', *, *, #866, .F. ) ;
#502 = CARTESIAN_POINT ( 'NONE',  ( -3.120626071653146649, 49.00000000000000000, 4.471016347907768029 ) ) ;
#503 = PRESENTATION_LAYER_ASSIGNMENT (  '', '', ( #4159 ) ) ;
#504 = CARTESIAN_POINT ( 'NONE',  ( 4.528983652092238188, 37.00000000000000000, 5.879373928346857348 ) ) ;
#505 = AXIS2_PLACEMENT_3D ( 'NONE', #4213, #3849, #899 ) ;
#506 = CARTESIAN_POINT ( 'NONE',  ( 0.000000000000000000, 0.000000000000000000, 17.00000000000000000 ) ) ;
#507 = PRODUCT ( 'start button', 'start button', '', ( #1061 ) ) ;
#508 = LINE ( 'NONE', #3408, #1317 ) ;
#509 = VECTOR ( 'NONE', #2115, 1000.000000000000000 ) ;
#510 = CARTESIAN_POINT ( 'NONE',  ( 0.7500000000000001110, 20.00000000000000000, 17.69999999999999929 ) ) ;
#511 = LINE ( 'NONE', #1671, #1812 ) ;
#512 = CARTESIAN_POINT ( 'NONE',  ( 0.000000000000000000, 20.00000000000000000, 17.69999999999999929 ) ) ;
#513 = ORIENTED_EDGE ( 'NONE', *, *, #1744, .T. ) ;
#514 = EDGE_CURVE ( 'NONE', #3612, #442, #4534, .T. ) ;
#515 = CARTESIAN_POINT ( 'NONE',  ( -3.889087296526001047, 34.17157287525380838, 6.110912703473974084 ) ) ;
#516 = EDGE_CURVE ( 'NONE', #1550, #1737, #1460, .T. ) ;
#517 = CARTESIAN_POINT ( 'NONE',  ( 26.49999999999999645, 0.5000000000000000000, 19.00000000000000000 ) ) ;
#518 = APPLICATION_CONTEXT ( 'automotive_design' ) ;
#519 = CARTESIAN_POINT ( 'NONE',  ( -18.29773070266338664, 23.77384460521234288, 7.963596978677149885 ) ) ;
#520 = AXIS2_PLACEMENT_3D ( 'NONE', #2929, #1829, #4028 ) ;
#521 = CARTESIAN_POINT ( 'NONE',  ( 0.7500000000000000000, -2.999999999999999556, 17.69999999999999929 ) ) ;
#522 = FILL_AREA_STYLE_COLOUR ( '', #3240 ) ;
#523 = DIRECTION ( 'NONE',  ( 0.000000000000000000, 1.000000000000000000, -0.000000000000000000 ) ) ;
#524 = ORIENTED_EDGE ( 'NONE', *, *, #4465, .F. ) ;
#525 = VERTEX_POINT ( 'NONE', #3971 ) ;
#526 = ORIENTED_EDGE ( 'NONE', *, *, #71, .F. ) ;
#527 = VECTOR ( 'NONE', #1706, 1000.000000000000000 ) ;
#528 = ORIENTED_EDGE ( 'NONE', *, *, #2213, .T. ) ;
#529 =( GEOMETRIC_REPRESENTATION_CONTEXT ( 3 ) GLOBAL_UNCERTAINTY_ASSIGNED_CONTEXT ( ( #79 ) ) GLOBAL_UNIT_ASSIGNED_CONTEXT ( ( #706, #2210, #4340 ) ) REPRESENTATION_CONTEXT ( 'NONE', 'WORKASPACE' ) );
#530 = FACE_OUTER_BOUND ( 'NONE', #2627, .T. ) ;
#531 = PRESENTATION_STYLE_ASSIGNMENT (( #2343 ) ) ;
#532 = CIRCLE ( 'NONE', #3102, 1.750000000000001554 ) ;
#533 = ORIENTED_EDGE ( 'NONE', *, *, #4639, .F. ) ;
#534 = DIRECTION ( 'NONE',  ( 0.000000000000000000, 1.000000000000000000, 0.000000000000000000 ) ) ;
#535 = PLANE ( 'NONE',  #4253 ) ;
#536 = FACE_BOUND ( 'NONE', #2532, .T. ) ;
#537 = ORIENTED_EDGE ( 'NONE', *, *, #1804, .F. ) ;
#538 = EDGE_CURVE ( 'NONE', #3343, #4108, #2239, .T. ) ;
#539 = VECTOR ( 'NONE', #2025, 1000.000000000000000 ) ;
#540 = CARTESIAN_POINT ( 'NONE',  ( 18.19536891688249369, 23.85222316637479523, 8.999999999999992895 ) ) ;
#541 = CARTESIAN_POINT ( 'NONE',  ( 0.000000000000000000, 0.000000000000000000, 18.19999999999999929 ) ) ;
#542 = EDGE_CURVE ( 'NONE', #3343, #1490, #1089, .T. ) ;
#543 = EDGE_CURVE ( 'NONE', #1651, #1279, #3319, .T. ) ;
#544 = DIRECTION ( 'NONE',  ( 0.000000000000000000, 0.000000000000000000, 1.000000000000000000 ) ) ;
#545 = CARTESIAN_POINT ( 'NONE',  ( -8.999999999999998224, 36.00000000000000711, 2.143131898507868051E-16 ) ) ;
#546 = PRODUCT_DEFINITION_SHAPE ( 'NONE', 'NONE',  #1816 ) ;
#547 = DIRECTION ( 'NONE',  ( 1.000000000000000000, 0.000000000000000000, 0.000000000000000000 ) ) ;
#548 = EDGE_LOOP ( 'NONE', ( #758, #4521, #1673, #3066 ) ) ;
#549 = EDGE_LOOP ( 'NONE', ( #476, #1269 ) ) ;
#550 = ORIENTED_EDGE ( 'NONE', *, *, #3857, .F. ) ;
#551 = ORIENTED_EDGE ( 'NONE', *, *, #253, .F. ) ;
#552 = LINE ( 'NONE', #1733, #440 ) ;
#553 = CIRCLE ( 'NONE', #2066, 1.000000000000000000 ) ;
#554 = CARTESIAN_POINT ( 'NONE',  ( -0.7500000000000001110, 1.299038105676658450, 17.69999999999999929 ) ) ;
#555 =( NAMED_UNIT ( * ) SI_UNIT ( $, .STERADIAN. ) SOLID_ANGLE_UNIT ( ) );
#556 = ORIENTED_EDGE ( 'NONE', *, *, #1846, .T. ) ;
#557 = VECTOR ( 'NONE', #4315, 1000.000000000000000 ) ;
#558 = CARTESIAN_POINT ( 'NONE',  ( 0.9958591954638854604, 37.00000000000000000, 14.40909090909091184 ) ) ;
#559 = CARTESIAN_POINT ( 'NONE',  ( -4.528983652092210654, 49.00000000000000000, 5.879373928346826261 ) ) ;
#560 = CARTESIAN_POINT ( 'NONE',  ( 5.409090909090911836, 37.00000000000000000, 8.004140804536053366 ) ) ;
#561 = ORIENTED_EDGE ( 'NONE', *, *, #1435, .T. ) ;
#562 = ADVANCED_FACE ( 'NONE', ( #416 ), #2265, .T. ) ;
#563 = CARTESIAN_POINT ( 'NONE',  ( 4.020538011569923144E-15, 41.00000000000000000, 4.999999999999990230 ) ) ;
#564 = EDGE_CURVE ( 'NONE', #213, #2091, #3689, .T. ) ;
#565 = CARTESIAN_POINT ( 'NONE',  ( 0.9958591954638856825, 49.00000000000000000, 14.40909090909091361 ) ) ;
#566 = AXIS2_PLACEMENT_3D ( 'NONE', #1204, #140, #4135 ) ;
#567 = CARTESIAN_POINT ( 'NONE',  ( -18.61638332444503519, 23.52555220673917447, 6.995423750305947763 ) ) ;
#568 = CARTESIAN_POINT ( 'NONE',  ( 3.469446951953614189E-15, 37.00000000000000711, 8.999999999999992895 ) ) ;
#569 = CARTESIAN_POINT ( 'NONE',  ( -26.00000000000000355, -1.592040838891558504E-15, 20.00000599999999906 ) ) ;
#570 = ORIENTED_EDGE ( 'NONE', *, *, #2926, .T. ) ;
#571 = AXIS2_PLACEMENT_3D ( 'NONE', #3387, #3314, #1154 ) ;
#572 = ORIENTED_EDGE ( 'NONE', *, *, #4588, .T. ) ;
#573 = ORIENTED_EDGE ( 'NONE', *, *, #86, .F. ) ;
#574 = VERTEX_POINT ( 'NONE', #3294 ) ;
#575 = LINE ( 'NONE', #4261, #2798 ) ;
#576 = PRODUCT_RELATED_PRODUCT_CATEGORY ( 'part', '', ( #206 ) ) ;
#577 = DIRECTION ( 'NONE',  ( 0.000000000000000000, 0.000000000000000000, -1.000000000000000000 ) ) ;
#578 =( GEOMETRIC_REPRESENTATION_CONTEXT ( 3 ) GLOBAL_UNCERTAINTY_ASSIGNED_CONTEXT ( ( #4075 ) ) GLOBAL_UNIT_ASSIGNED_CONTEXT ( ( #32, #1473, #1933 ) ) REPRESENTATION_CONTEXT ( 'NONE', 'WORKASPACE' ) );
#579 = EDGE_CURVE ( 'NONE', #3730, #2339, #1566, .T. ) ;
#580 = DIRECTION ( 'NONE',  ( 0.000000000000000000, 1.000000000000000000, 0.000000000000000000 ) ) ;
#581 = DIRECTION ( 'NONE',  ( 0.000000000000000000, 0.000000000000000000, -1.000000000000000000 ) ) ;
#582 = MECHANICAL_DESIGN_GEOMETRIC_PRESENTATION_REPRESENTATION (  '', ( #2698 ), #3535 ) ;
#583 = EDGE_CURVE ( 'NONE', #763, #2091, #94, .T. ) ;
#584 = DIRECTION ( 'NONE',  ( -0.000000000000000000, -1.000000000000000000, -0.000000000000000000 ) ) ;
#585 = DIRECTION ( 'NONE',  ( 0.000000000000000000, 0.000000000000000000, 1.000000000000000000 ) ) ;
#586 = CARTESIAN_POINT ( 'NONE',  ( 3.469446951953614189E-15, 30.00000000000000355, 8.999999999999992895 ) ) ;
#587 = PRESENTATION_LAYER_ASSIGNMENT (  '', '', ( #2698 ) ) ;
#588 = EDGE_LOOP ( 'NONE', ( #1122, #2733, #4479, #3461 ) ) ;
#589 = VECTOR ( 'NONE', #847, 1000.000000000000000 ) ;
#590 = APPLICATION_CONTEXT ( 'automotive_design' ) ;
#591 = CARTESIAN_POINT ( 'NONE',  ( -14.84924240491753089, 20.50609665440985552, 8.999999999999992895 ) ) ;
#592 = MECHANICAL_DESIGN_GEOMETRIC_PRESENTATION_REPRESENTATION (  '', ( #1718 ), #2469 ) ;
#593 = CARTESIAN_POINT ( 'NONE',  ( 19.25985638980603554, 23.00200370561274354, 12.01100206247544300 ) ) ;
#594 = DIRECTION ( 'NONE',  ( -1.000000000000000000, -0.000000000000000000, -0.000000000000000000 ) ) ;
#595 = CARTESIAN_POINT ( 'NONE',  ( -21.58204166899923138, 20.83941891177991224, 5.025993266704736229 ) ) ;
#596 = DIRECTION ( 'NONE',  ( 0.000000000000000000, 0.000000000000000000, -1.000000000000000000 ) ) ;
#597 = CARTESIAN_POINT ( 'NONE',  ( 3.889087296526035242, 49.00000000000000000, 5.110912703473999841 ) ) ;
#598 = ORIENTED_EDGE ( 'NONE', *, *, #3273, .T. ) ;
#599 = EDGE_LOOP ( 'NONE', ( #237, #2178, #2583, #28 ) ) ;
#600 = ORIENTED_EDGE ( 'NONE', *, *, #1650, .T. ) ;
#601 = CARTESIAN_POINT ( 'NONE',  ( 3.469446951953614189E-15, 49.00000000000000000, 8.999999999999992895 ) ) ;
#602 = CARTESIAN_POINT ( 'NONE',  ( -27.10000000000000497, 0.6000000000000000888, 19.59999999999999787 ) ) ;
#603 = ADVANCED_FACE ( 'NONE', ( #1206 ), #2987, .F. ) ;
#604 =( NAMED_UNIT ( * ) SI_UNIT ( $, .STERADIAN. ) SOLID_ANGLE_UNIT ( ) );
#605 = DIRECTION ( 'NONE',  ( -0.000000000000000000, 1.000000000000000000, -0.000000000000000000 ) ) ;
#606=STYLED_ITEM('',(#4736),#2883);
#607 = CARTESIAN_POINT ( 'NONE',  ( 0.7500000000000000000, -1.299038105676658450, 18.19999999999999929 ) ) ;
#608 = LINE ( 'NONE', #3479, #393 ) ;
#609 = COLOUR_RGB ( '',0.8941176470588234615, 0.8941176470588234615, 0.8941176470588234615 ) ;
#610 = DIRECTION ( 'NONE',  ( 0.000000000000000000, 0.000000000000000000, 1.000000000000000000 ) ) ;
#611 = EDGE_CURVE ( 'NONE', #4468, #4460, #1182, .T. ) ;
#612 = CARTESIAN_POINT ( 'NONE',  ( -25.99519186311192342, -0.5000000000000000000, 19.50000000000000000 ) ) ;
#613 = EDGE_CURVE ( 'NONE', #1651, #574, #4113, .T. ) ;
#614 = VERTEX_POINT ( 'NONE', #1484 ) ;
#615 = DIRECTION ( 'NONE',  ( 8.921435019309286191E-15, 1.000000000000000000, 0.000000000000000000 ) ) ;
#616 = CARTESIAN_POINT ( 'NONE',  ( -2.007411586324088226, 29.93355017142139118, 12.46960170373642640 ) ) ;
#617 = DIRECTION ( 'NONE',  ( 0.000000000000000000, 0.000000000000000000, 1.000000000000000000 ) ) ;
#618 = CARTESIAN_POINT ( 'NONE',  ( -23.85222316637485562, 18.19536891688241198, 8.999999999999992895 ) ) ;
#619 = DIRECTION ( 'NONE',  ( 1.000000000000000000, 0.000000000000000000, 0.000000000000000000 ) ) ;
#620 = ADVANCED_FACE ( 'NONE', ( #67 ), #1945, .T. ) ;
#621 = FACE_OUTER_BOUND ( 'NONE', #395, .T. ) ;
#622 = ORIENTED_EDGE ( 'NONE', *, *, #410, .T. ) ;
#623 = ORIENTED_EDGE ( 'NONE', *, *, #3700, .F. ) ;
#624 = ADVANCED_FACE ( 'NONE', ( #2648 ), #2287, .T. ) ;
#625 = CARTESIAN_POINT ( 'NONE',  ( 25.99519186311192342, -0.5000000000000000000, 19.50000000000000000 ) ) ;
#626 = CARTESIAN_POINT ( 'NONE',  ( -0.9958591954639161026, 37.00000000000000000, 3.590909090909080170 ) ) ;
#627 =( NAMED_UNIT ( * ) SI_UNIT ( $, .STERADIAN. ) SOLID_ANGLE_UNIT ( ) );
#628 = DIRECTION ( 'NONE',  ( 0.000000000000000000, 0.000000000000000000, 1.000000000000000000 ) ) ;
#629 = CARTESIAN_POINT ( 'NONE',  ( 8.377607117416813409, 24.67207871933482366, 20.00001200000000523 ) ) ;
#630 = AXIS2_PLACEMENT_3D ( 'NONE', #850, #2727, #2290 ) ;
#631 = CIRCLE ( 'NONE', #2748, 5.500000000000000000 ) ;
#632 = DIRECTION ( 'NONE',  ( -0.000000000000000000, 1.000000000000000000, -0.000000000000000000 ) ) ;
#633 = CARTESIAN_POINT ( 'NONE',  ( 26.49999999999999645, 0.5000000000000000000, 19.00000000000000000 ) ) ;
#634 = CARTESIAN_POINT ( 'NONE',  ( 3.796098697355190676, 29.75902942016942987, 7.712254142552557923 ) ) ;
#635 = CIRCLE ( 'NONE', #3283, 1.500000000000000222 ) ;
#636 = EDGE_LOOP ( 'NONE', ( #2161, #3608, #3305, #4453 ) ) ;
#637 = SURFACE_STYLE_USAGE ( .BOTH. , #4658 ) ;
#638 = PRODUCT_RELATED_PRODUCT_CATEGORY ( 'part', '', ( #2787 ) ) ;
#639 = CIRCLE ( 'NONE', #3339, 26.00000000000000355 ) ;
#640 = DIRECTION ( 'NONE',  ( 0.000000000000000000, 0.000000000000000000, -1.000000000000000000 ) ) ;
#641 = DIRECTION ( 'NONE',  ( -1.000000000000000000, 0.000000000000000000, 0.000000000000000000 ) ) ;
#642 = CARTESIAN_POINT ( 'NONE',  ( 3.469446951953614189E-15, 37.00000000000000711, 4.999999999999992006 ) ) ;
#643 = CARTESIAN_POINT ( 'NONE',  ( 0.5000000000000000000, 0.000000000000000000, 20.00000000000000000 ) ) ;
#644 = DIRECTION ( 'NONE',  ( 1.000000000000000000, 0.000000000000000000, 0.000000000000000000 ) ) ;
#645 = ORIENTED_EDGE ( 'NONE', *, *, #2272, .F. ) ;
#646 = ORIENTED_EDGE ( 'NONE', *, *, #4119, .F. ) ;
#647 = CIRCLE ( 'NONE', #3292, 26.00000000000000355 ) ;
#648 = CARTESIAN_POINT ( 'NONE',  ( 27.09999999999999787, 0.6000000000000000888, 19.59999999999999787 ) ) ;
#649 = DIRECTION ( 'NONE',  ( 0.000000000000000000, 0.000000000000000000, -1.000000000000000000 ) ) ;
#650 = CIRCLE ( 'NONE', #4445, 26.00000000000000355 ) ;
#651 =( LENGTH_UNIT ( ) NAMED_UNIT ( * ) SI_UNIT ( .MILLI., .METRE. ) );
#652 = CARTESIAN_POINT ( 'NONE',  ( 26.49999999999999645, 0.5000000000000000000, 19.50000000000000000 ) ) ;
#653 = CARTESIAN_POINT ( 'NONE',  ( 3.959305671612554781E-15, 43.00000000000000000, 12.99999999999999289 ) ) ;
#654 = DIRECTION ( 'NONE',  ( 0.000000000000000000, 0.000000000000000000, 1.000000000000000000 ) ) ;
#655 = CARTESIAN_POINT ( 'NONE',  ( 12.00000000000000178, 36.00000000000000000, 0.000000000000000000 ) ) ;
#656 =( GEOMETRIC_REPRESENTATION_CONTEXT ( 3 ) GLOBAL_UNCERTAINTY_ASSIGNED_CONTEXT ( ( #1169 ) ) GLOBAL_UNIT_ASSIGNED_CONTEXT ( ( #3518, #1074, #4331 ) ) REPRESENTATION_CONTEXT ( 'NONE', 'WORKASPACE' ) );
#657 =( NAMED_UNIT ( * ) SI_UNIT ( $, .STERADIAN. ) SOLID_ANGLE_UNIT ( ) );
#658 = VECTOR ( 'NONE', #781, 1000.000000000000000 ) ;
#659 = DIRECTION ( 'NONE',  ( 0.000000000000000000, -0.000000000000000000, 1.000000000000000000 ) ) ;
#660 = SURFACE_SIDE_STYLE ('',( #3422 ) ) ;
#661 = DIRECTION ( 'NONE',  ( 0.000000000000000000, 0.000000000000000000, 1.000000000000000000 ) ) ;
#662 = AXIS2_PLACEMENT_3D ( 'NONE', #4517, #1950, #1265 ) ;
#663 = AXIS2_PLACEMENT_3D ( 'NONE', #685, #3576, #3286 ) ;
#664 = ADVANCED_FACE ( 'NONE', ( #491 ), #1842, .T. ) ;
#665 = CARTESIAN_POINT ( 'NONE',  ( -23.52449179749635277, 18.61772044889870159, 6.992605352578565636 ) ) ;
#666 = CARTESIAN_POINT ( 'NONE',  ( -3.889087296526055226, 34.17157287525380838, 12.88908729652595753 ) ) ;
#667 = LINE ( 'NONE', #1046, #131 ) ;
#668 = VERTEX_POINT ( 'NONE', #3651 ) ;
#669 = ORIENTED_EDGE ( 'NONE', *, *, #1744, .F. ) ;
#670 = FACE_OUTER_BOUND ( 'NONE', #858, .T. ) ;
#671 = DIRECTION ( 'NONE',  ( -0.000000000000000000, -1.000000000000000000, -0.000000000000000000 ) ) ;
#672 = FILL_AREA_STYLE ('',( #2807 ) ) ;
#673 = DIRECTION ( 'NONE',  ( -0.000000000000000000, 0.000000000000000000, 1.000000000000000000 ) ) ;
#674 = CARTESIAN_POINT ( 'NONE',  ( 24.00000000000000355, 0.000000000000000000, 17.00000000000000000 ) ) ;
#675 = ORIENTED_EDGE ( 'NONE', *, *, #4119, .T. ) ;
#676 = DIRECTION ( 'NONE',  ( 1.000000000000000000, 0.000000000000000000, 0.000000000000000000 ) ) ;
#677 = CIRCLE ( 'NONE', #3941, 1.500000000000000222 ) ;
#678 = DIRECTION ( 'NONE',  ( 0.000000000000000000, 0.000000000000000000, 1.000000000000000000 ) ) ;
#679 = DIRECTION ( 'NONE',  ( 1.000000000000000000, 0.000000000000000000, 0.000000000000000000 ) ) ;
#680 = AXIS2_PLACEMENT_3D ( 'NONE', #2681, #1906, #2998 ) ;
#681 = CYLINDRICAL_SURFACE ( 'NONE', #1102, 0.7500000000000001110 ) ;
#682 = AXIS2_PLACEMENT_3D ( 'NONE', #4584, #4229, #972 ) ;
#683 = CARTESIAN_POINT ( 'NONE',  ( 3.809991693235077026, 31.40492942523385267, 7.766500207085086593 ) ) ;
#684 = PRODUCT_CONTEXT ( 'NONE', #3739, 'mechanical' ) ;
#685 = CARTESIAN_POINT ( 'NONE',  ( 3.469446951953614189E-15, 33.00000000000000000, 8.999999999999992895 ) ) ;
#686 = VECTOR ( 'NONE', #1993, 1000.000000000000000 ) ;
#687 = EDGE_CURVE ( 'NONE', #1161, #2307, #2576, .T. ) ;
#688 = EDGE_CURVE ( 'NONE', #2966, #22, #4307, .T. ) ;
#689 = FACE_OUTER_BOUND ( 'NONE', #2400, .T. ) ;
#690 = CARTESIAN_POINT ( 'NONE',  ( 8.999999999999980460, 32.99999999999999289, -1.749999999999999778 ) ) ;
#691 = DIRECTION ( 'NONE',  ( 1.000000000000000000, 0.000000000000000000, 0.000000000000000000 ) ) ;
#692 = AXIS2_PLACEMENT_3D ( 'NONE', #597, #3115, #4195 ) ;
#693 = EDGE_CURVE ( 'NONE', #1443, #1195, #4565, .T. ) ;
#694 = ORIENTED_EDGE ( 'NONE', *, *, #4339, .F. ) ;
#695 = EDGE_LOOP ( 'NONE', ( #214, #1153, #2156, #1634, #75 ) ) ;
#696 = EDGE_CURVE ( 'NONE', #4356, #1339, #886, .T. ) ;
#697 = LINE ( 'NONE', #3186, #1821 ) ;
#698 = VECTOR ( 'NONE', #1121, 1000.000000000000000 ) ;
#699 = DIRECTION ( 'NONE',  ( 0.000000000000000000, 0.000000000000000000, 1.000000000000000000 ) ) ;
#700 = EDGE_LOOP ( 'NONE', ( #4101, #4550, #228, #2693, #3793 ) ) ;
#701 = CARTESIAN_POINT ( 'NONE',  ( 3.959305671612554781E-15, 37.00000000000000711, 12.99999999999999289 ) ) ;
#702 = CARTESIAN_POINT ( 'NONE',  ( 9.000000000000003553, 36.00000000000000000, 0.000000000000000000 ) ) ;
#703 = LINE ( 'NONE', #1079, #900 ) ;
#704 = CARTESIAN_POINT ( 'NONE',  ( 3.872997316437435167, 29.74899170013632954, 7.966596725458382267 ) ) ;
#705 = CIRCLE ( 'NONE', #1311, 0.7500000000000001110 ) ;
#706 =( LENGTH_UNIT ( ) NAMED_UNIT ( * ) SI_UNIT ( .MILLI., .METRE. ) );
#707 = VECTOR ( 'NONE', #1175, 1000.000000000000000 ) ;
#708 = B_SPLINE_CURVE_WITH_KNOTS ( 'NONE', 3,
 ( #3293, #846, #2286, #1159, #3745, #490, #823, #2264, #4490, #41, #2216, #1864, #3670, #1604, #4165, #162, #3129, #3463, #2745, #2796, #4252, #2351, #4610, #898, #2425, #2037, #3823, #616, #2328, #1989, #993, #948, #2770, #3438 ),
 .UNSPECIFIED., .F., .F.,
 ( 4, 2, 2, 2, 2, 2, 2, 2, 2, 2, 2, 2, 2, 2, 2, 2, 4 ),
 ( 0.000000000000000000, 0.0007824850735655043557, 0.001564970147131008711, 0.002347455220696513176, 0.003129940294262017423, 0.003912425367827521670, 0.004694910441393026351, 0.005477395514958530165, 0.006259880588524034846, 0.007042365662089539527, 0.007824850735655043341, 0.008607335809220547154, 0.009389820882786052703, 0.01017230595635155652, 0.01095479102991706033, 0.01173727610348256588, 0.01251976117704806969 ),
 .UNSPECIFIED. ) ;
#709 = FACE_BOUND ( 'NONE', #2678, .T. ) ;
#710 = APPLICATION_PROTOCOL_DEFINITION ( 'draft international standard', 'automotive_design', 1998, #4258 ) ;
#711 = EDGE_CURVE ( 'NONE', #3855, #2686, #2311, .T. ) ;
#712 = CARTESIAN_POINT ( 'NONE',  ( -27.10000000000000497, -0.5999999999999998668, 19.00000000000000000 ) ) ;
#713 = CARTESIAN_POINT ( 'NONE',  ( 10.25000000000001954, 44.99999999999999289, 2.143131898507868051E-16 ) ) ;
#714 = DIRECTION ( 'NONE',  ( 0.000000000000000000, 0.000000000000000000, 1.000000000000000000 ) ) ;
#715 = VERTEX_POINT ( 'NONE', #3488 ) ;
#716 = EDGE_LOOP ( 'NONE', ( #908, #4000 ) ) ;
#717 = CARTESIAN_POINT ( 'NONE',  ( -5.409090909090905619, 33.00000000000000000, 10.99999999999999289 ) ) ;
#718 = CARTESIAN_POINT ( 'NONE',  ( 3.469446951953614189E-15, 41.00000000000000000, 8.999999999999992895 ) ) ;
#719 = EDGE_LOOP ( 'NONE', ( #3325, #1461, #3259, #694 ) ) ;
#720 = ORIENTED_EDGE ( 'NONE', *, *, #4282, .F. ) ;
#721 = CARTESIAN_POINT ( 'NONE',  ( 3.403349963601422168, 25.83240171513484285, 20.00001200000000523 ) ) ;
#722 = EDGE_CURVE ( 'NONE', #4523, #3514, #2026, .T. ) ;
#723 = DIRECTION ( 'NONE',  ( 0.000000000000000000, 0.000000000000000000, 1.000000000000000000 ) ) ;
#724 = EDGE_CURVE ( 'NONE', #2854, #2731, #4586, .T. ) ;
#725 = CARTESIAN_POINT ( 'NONE',  ( -0.5000000000000000000, 0.000000000000000000, 19.50000000000000000 ) ) ;
#726 = DIRECTION ( 'NONE',  ( 1.000000000000000000, 0.000000000000000000, 0.000000000000000000 ) ) ;
#727 = EDGE_CURVE ( 'NONE', #442, #499, #2378, .T. ) ;
#728 = FILL_AREA_STYLE_COLOUR ( '', #2564 ) ;
#729 = AXIS2_PLACEMENT_3D ( 'NONE', #506, #221, #3815 ) ;
#730 = DIRECTION ( 'NONE',  ( 1.000000000000000000, 0.000000000000000000, -0.000000000000000000 ) ) ;
#731 = CIRCLE ( 'NONE', #3389, 8.000000000000000000 ) ;
#732 = CYLINDRICAL_SURFACE ( 'NONE', #3891, 0.7500000000000001110 ) ;
#733 = DIRECTION ( 'NONE',  ( 5.782411586589374402E-16, -1.000000000000000000, 0.000000000000000000 ) ) ;
#734 = CARTESIAN_POINT ( 'NONE',  ( -3.523144759583856978, 33.65295909972188326, 7.105089090000585195 ) ) ;
#735 = VECTOR ( 'NONE', #2831, 1000.000000000000000 ) ;
#736 = ORIENTED_EDGE ( 'NONE', *, *, #2437, .F. ) ;
#737 = EDGE_LOOP ( 'NONE', ( #3427, #3754, #3126, #2585 ) ) ;
#738 = CARTESIAN_POINT ( 'NONE',  ( -3.575465955037816723, 32.10687100738867628, 7.205771075917310142 ) ) ;
#739 = FILL_AREA_STYLE ('',( #3997 ) ) ;
#740 = DIRECTION ( 'NONE',  ( 1.000000000000000000, 0.000000000000000000, 0.000000000000000000 ) ) ;
#741 = VERTEX_POINT ( 'NONE', #2403 ) ;
#742 = VERTEX_POINT ( 'NONE', #209 ) ;
#743 = ORIENTED_EDGE ( 'NONE', *, *, #50, .F. ) ;
#744 = DIRECTION ( 'NONE',  ( -0.000000000000000000, -0.000000000000000000, -1.000000000000000000 ) ) ;
#745 = EDGE_CURVE ( 'NONE', #378, #1543, #4609, .T. ) ;
#746 = PRESENTATION_STYLE_ASSIGNMENT (( #1882 ) ) ;
#747 = EDGE_LOOP ( 'NONE', ( #2220, #2706, #1118, #1381 ) ) ;
#748 = SURFACE_SIDE_STYLE ('',( #2910 ) ) ;
#749 = EDGE_CURVE ( 'NONE', #1146, #1098, #2012, .T. ) ;
#750 = VECTOR ( 'NONE', #3405, 1000.000000000000000 ) ;
#751 = EDGE_CURVE ( 'NONE', #954, #2636, #2353, .T. ) ;
#752 = CARTESIAN_POINT ( 'NONE',  ( 3.501320667853366153, 32.47456368659583603, 10.93433813232663887 ) ) ;
#753 = SHAPE_DEFINITION_REPRESENTATION ( #1564, #773 ) ;
#754=STYLED_ITEM('',(#4729),#2889);
#755 = DIRECTION ( 'NONE',  ( -1.000000000000000000, 0.000000000000000000, 0.000000000000000000 ) ) ;
#756 = CARTESIAN_POINT ( 'NONE',  ( 0.7500000000000001110, 9.184850993605150903E-17, 15.00000000000000178 ) ) ;
#757 = DIRECTION ( 'NONE',  ( 0.000000000000000000, 0.000000000000000000, -1.000000000000000000 ) ) ;
#758 = ORIENTED_EDGE ( 'NONE', *, *, #1941, .F. ) ;
#759 = ORIENTED_EDGE ( 'NONE', *, *, #4685, .T. ) ;
#760 = DIRECTION ( 'NONE',  ( 0.000000000000000000, 0.000000000000000000, 1.000000000000000000 ) ) ;
#761 = EDGE_CURVE ( 'NONE', #4484, #1375, #3922, .T. ) ;
#762 = DIRECTION ( 'NONE',  ( 1.000000000000000000, -8.560005772541128451E-15, 0.000000000000000000 ) ) ;
#763 = VERTEX_POINT ( 'NONE', #565 ) ;
#764 = ORIENTED_EDGE ( 'NONE', *, *, #2794, .T. ) ;
#765 = VERTEX_POINT ( 'NONE', #1699 ) ;
#766 = EDGE_CURVE ( 'NONE', #1507, #1468, #1480, .T. ) ;
#767 = CARTESIAN_POINT ( 'NONE',  ( -1.734723475976807094E-15, 45.00000000000000000, 2.143131898507868051E-16 ) ) ;
#768 = AXIS2_PLACEMENT_3D ( 'NONE', #3232, #762, #3279 ) ;
#769 = CARTESIAN_POINT ( 'NONE',  ( -18.84808613845423508, 23.34033764136069422, 11.44520879210846687 ) ) ;
#770 = DIRECTION ( 'NONE',  ( -0.000000000000000000, -0.000000000000000000, -1.000000000000000000 ) ) ;
#771 = CARTESIAN_POINT ( 'NONE',  ( 15.85973458909327505, -20.67279826512041296, 20.00001199999999457 ) ) ;
#772 = ORIENTED_EDGE ( 'NONE', *, *, #1404, .T. ) ;
#773 = SHAPE_REPRESENTATION ( 'minute hand', ( #2928 ), #3769 ) ;
#774 = FACE_OUTER_BOUND ( 'NONE', #4403, .T. ) ;
#775 = CARTESIAN_POINT ( 'NONE',  ( -8.000000000000000000, 10.00000000000000178, 15.00000000000000178 ) ) ;
#776 = AXIS2_PLACEMENT_3D ( 'NONE', #3918, #3873, #255 ) ;
#777 = EDGE_CURVE ( 'NONE', #1588, #3297, #4191, .T. ) ;
#778 = EDGE_CURVE ( 'NONE', #956, #1513, #731, .T. ) ;
#779 = DIRECTION ( 'NONE',  ( -0.000000000000000000, -0.000000000000000000, 1.000000000000000000 ) ) ;
#780 = CARTESIAN_POINT ( 'NONE',  ( -13.75000000000000178, 36.00000000000001421, 0.000000000000000000 ) ) ;
#781 = DIRECTION ( 'NONE',  ( 0.000000000000000000, 0.000000000000000000, 1.000000000000000000 ) ) ;
#782 = CIRCLE ( 'NONE', #2359, 5.500000000000000000 ) ;
#783 = ORIENTED_EDGE ( 'NONE', *, *, #925, .T. ) ;
#784 = ORIENTED_EDGE ( 'NONE', *, *, #2861, .T. ) ;
#785 = CARTESIAN_POINT ( 'NONE',  ( -3.706735793540070656, 31.67823920415836625, 7.493470964888215846 ) ) ;
#786 = VERTEX_POINT ( 'NONE', #4232 ) ;
#787 = EDGE_LOOP ( 'NONE', ( #3435, #2481, #1946, #2209, #849 ) ) ;
#788 = VERTEX_POINT ( 'NONE', #975 ) ;
#789 = DIRECTION ( 'NONE',  ( -0.000000000000000000, -0.000000000000000000, 1.000000000000000000 ) ) ;
#790 = DIRECTION ( 'NONE',  ( 0.000000000000000000, -0.000000000000000000, 1.000000000000000000 ) ) ;
#791 = CARTESIAN_POINT ( 'NONE',  ( 0.000000000000000000, 6.000000000000000000, 19.50000000000000000 ) ) ;
#792 = CARTESIAN_POINT ( 'NONE',  ( 0.5000000000000001110, 6.123233995736767268E-17, 16.00000000000000000 ) ) ;
#793 = EDGE_LOOP ( 'NONE', ( #1095, #3584 ) ) ;
#794 = AXIS2_PLACEMENT_3D ( 'NONE', #465, #2986, #2671 ) ;
#795 = PLANE ( 'NONE',  #1205 ) ;
#796 = DIRECTION ( 'NONE',  ( 1.000000000000000000, 0.000000000000000000, 0.000000000000000000 ) ) ;
#797 = AXIS2_PLACEMENT_3D ( 'NONE', #4318, #1787, #3597 ) ;
#798 = MECHANICAL_DESIGN_GEOMETRIC_PRESENTATION_REPRESENTATION (  '', ( #3759 ), #4070 ) ;
#799 = DIRECTION ( 'NONE',  ( 1.000000000000000000, 0.000000000000000000, 0.000000000000000000 ) ) ;
#800 = DIRECTION ( 'NONE',  ( 0.000000000000000000, 0.000000000000000000, 1.000000000000000000 ) ) ;
#801 = DIRECTION ( 'NONE',  ( -0.000000000000000000, -1.000000000000000000, -0.000000000000000000 ) ) ;
#802 = ORIENTED_EDGE ( 'NONE', *, *, #1661, .F. ) ;
#803 = VERTEX_POINT ( 'NONE', #3872 ) ;
#804 = EDGE_CURVE ( 'NONE', #85, #3729, #1345, .T. ) ;
#805 = PLANE ( 'NONE',  #1597 ) ;
#806 = FACE_OUTER_BOUND ( 'NONE', #1194, .T. ) ;
#807 = ADVANCED_FACE ( 'NONE', ( #2697 ), #252, .T. ) ;
#808 = VECTOR ( 'NONE', #923, 1000.000000000000000 ) ;
#809 = CARTESIAN_POINT ( 'NONE',  ( -0.7500000000000001110, 20.00000000000000000, 17.69999999999999929 ) ) ;
#810 = ORIENTED_EDGE ( 'NONE', *, *, #1129, .F. ) ;
#811 = ORIENTED_EDGE ( 'NONE', *, *, #4287, .T. ) ;
#812 = ORIENTED_EDGE ( 'NONE', *, *, #1517, .F. ) ;
#813 = CARTESIAN_POINT ( 'NONE',  ( -5.409090909090905619, 33.00000000000000000, 8.999999999999992895 ) ) ;
#814 = CARTESIAN_POINT ( 'NONE',  ( -21.40213195504977861, 21.02424009228906243, 12.99981531858142425 ) ) ;
#815 = FILL_AREA_STYLE ('',( #4007 ) ) ;
#816 = VERTEX_POINT ( 'NONE', #949 ) ;
#817 = CARTESIAN_POINT ( 'NONE',  ( -25.99307600111999150, 0.5999999999999998668, 19.59999999999999787 ) ) ;
#818 = DIRECTION ( 'NONE',  ( -0.000000000000000000, -0.000000000000000000, -1.000000000000000000 ) ) ;
#819 = CONTEXT_DEPENDENT_SHAPE_REPRESENTATION ( #274, #4659 ) ;
#820 = ADVANCED_FACE ( 'NONE', ( #2331 ), #3803, .T. ) ;
#821 = CIRCLE ( 'NONE', #2478, 5.000000000000002665 ) ;
#822 = CARTESIAN_POINT ( 'NONE',  ( 18.19536891688249369, 23.85222316637479523, 8.999999999999992895 ) ) ;
#823 = CARTESIAN_POINT ( 'NONE',  ( -2.004590926901224535, 29.93374515888019971, 5.528701699505815803 ) ) ;
#824 = VECTOR ( 'NONE', #4005, 1000.000000000000000 ) ;
#825 = CARTESIAN_POINT ( 'NONE',  ( -3.775090262067420710, 34.50279623606592594, 10.32592777499123748 ) ) ;
#826 = EDGE_LOOP ( 'NONE', ( #4327, #1268 ) ) ;
#827 = ORIENTED_EDGE ( 'NONE', *, *, #3495, .T. ) ;
#828 = EDGE_CURVE ( 'NONE', #3515, #1443, #3541, .T. ) ;
#829 = PRESENTATION_LAYER_ASSIGNMENT (  '', '', ( #1889 ) ) ;
#830 = DIRECTION ( 'NONE',  ( 1.000000000000000000, 0.000000000000000000, 0.000000000000000000 ) ) ;
#831 = CARTESIAN_POINT ( 'NONE',  ( 0.000000000000000000, 0.000000000000000000, 19.50000000000000000 ) ) ;
#832 = CARTESIAN_POINT ( 'NONE',  ( 0.5000000000000000000, 0.000000000000000000, 19.50000000000000000 ) ) ;
#833 = ORIENTED_EDGE ( 'NONE', *, *, #2217, .F. ) ;
#834 = VERTEX_POINT ( 'NONE', #3943 ) ;
#835 = ORIENTED_EDGE ( 'NONE', *, *, #777, .T. ) ;
#836 = ORIENTED_EDGE ( 'NONE', *, *, #2413, .T. ) ;
#837 = UNCERTAINTY_MEASURE_WITH_UNIT (LENGTH_MEASURE( 1.000000000000000082E-05 ), #4288, 'distance_accuracy_value', 'NONE');
#838 = DIRECTION ( 'NONE',  ( 1.000000000000000000, 0.000000000000000000, 0.000000000000000000 ) ) ;
#839 = PRODUCT_DEFINITION ( 'UNKNOWN', '', #2243, #1713 ) ;
#840 = CARTESIAN_POINT ( 'NONE',  ( -23.00200370561280749, 19.25985638980596093, 12.01100206247544300 ) ) ;
#841 = LINE ( 'NONE', #58, #197 ) ;
#842 = EDGE_LOOP ( 'NONE', ( #3173, #371, #223, #2579 ) ) ;
#843 = AXIS2_PLACEMENT_3D ( 'NONE', #2460, #2508, #3928 ) ;
#844 = DIRECTION ( 'NONE',  ( 0.000000000000000000, -1.000000000000000000, 0.000000000000000000 ) ) ;
#845 = CARTESIAN_POINT ( 'NONE',  ( 3.464101615137758827, 32.86736921533707800, 10.99999999999999822 ) ) ;
#846 = CARTESIAN_POINT ( 'NONE',  ( -0.2646063747045178660, 30.00000000000000000, 4.999999999999992895 ) ) ;
#847 = DIRECTION ( 'NONE',  ( 1.000000000000000000, -0.000000000000000000, -0.000000000000000000 ) ) ;
#848 = AXIS2_PLACEMENT_3D ( 'NONE', #3084, #1630, #544 ) ;
#849 = ORIENTED_EDGE ( 'NONE', *, *, #1941, .T. ) ;
#850 = CARTESIAN_POINT ( 'NONE',  ( -27.10000000000000497, -0.5999999999999998668, 19.59999999999999787 ) ) ;
#851 = CARTESIAN_POINT ( 'NONE',  ( -3.889087296526001047, 37.00000000000000000, 6.110912703473974084 ) ) ;
#852 = AXIS2_PLACEMENT_3D ( 'NONE', #4182, #2344, #156 ) ;
#853 = AXIS2_PLACEMENT_3D ( 'NONE', #455, #2640, #4104 ) ;
#854 = CARTESIAN_POINT ( 'NONE',  ( 3.120626071653123557, 49.00000000000000000, 13.52898365209223996 ) ) ;
#855 = ORIENTED_EDGE ( 'NONE', *, *, #2538, .T. ) ;
#856 = ORIENTED_EDGE ( 'NONE', *, *, #4405, .T. ) ;
#857 = EDGE_LOOP ( 'NONE', ( #3821, #3714, #2924, #2649 ) ) ;
#858 = EDGE_LOOP ( 'NONE', ( #109, #134, #2567, #1803 ) ) ;
#859 = DIRECTION ( 'NONE',  ( -1.428364815747576977E-15, -1.000000000000000000, 0.000000000000000000 ) ) ;
#860 = UNCERTAINTY_MEASURE_WITH_UNIT (LENGTH_MEASURE( 1.000000000000000082E-05 ), #447, 'distance_accuracy_value', 'NONE');
#861 = AXIS2_PLACEMENT_3D ( 'NONE', #1053, #2489, #4334 ) ;
#862 = DIRECTION ( 'NONE',  ( 0.000000000000000000, 0.000000000000000000, 1.000000000000000000 ) ) ;
#863 = EDGE_CURVE ( 'NONE', #4361, #4498, #4302, .T. ) ;
#864 = EDGE_CURVE ( 'NONE', #668, #1336, #2102, .T. ) ;
#865 = DIRECTION ( 'NONE',  ( -0.000000000000000000, 1.000000000000000000, -0.000000000000000000 ) ) ;
#866 = EDGE_CURVE ( 'NONE', #4468, #883, #1530, .T. ) ;
#867 = DIRECTION ( 'NONE',  ( 0.000000000000000000, 0.000000000000000000, 1.000000000000000000 ) ) ;
#868 = DIRECTION ( 'NONE',  ( -0.000000000000000000, -0.000000000000000000, -1.000000000000000000 ) ) ;
#869 = ORIENTED_EDGE ( 'NONE', *, *, #722, .T. ) ;
#870 = AXIS2_PLACEMENT_3D ( 'NONE', #231, #973, #4564 ) ;
#871 = B_SPLINE_CURVE_WITH_KNOTS ( 'NONE', 3,
 ( #540, #1305, #4536, #1281, #4211, #251, #1652, #1969, #1353, #593, #3416, #208, #2011, #2724, #3109, #2376, #3847, #1330, #4231, #3870, #1698, #1085, #4341, #3986, #343, #1745, #2911, #4635, #2104, #2520, #1722, #3624, #2497, #3529 ),
 .UNSPECIFIED., .F., .F.,
 ( 4, 2, 2, 2, 2, 2, 2, 2, 2, 2, 2, 2, 2, 2, 2, 2, 4 ),
 ( 0.01251975318912558477, 0.01330204881184919585, 0.01408434443457280694, 0.01486664005729641802, 0.01564893568002002910, 0.01643123130274364019, 0.01721352692546725127, 0.01799582254819086236, 0.01877811817091447344, 0.01956041379363808452, 0.02034270941636169561, 0.02112500503908530669, 0.02190730066180891430, 0.02268959628453252539, 0.02347189190725613647, 0.02425418752997974756, 0.02503648315270335864 ),
 .UNSPECIFIED. ) ;
#872 = VECTOR ( 'NONE', #2620, 1000.000000000000000 ) ;
#873 = DIRECTION ( 'NONE',  ( -0.000000000000000000, 1.000000000000000000, -0.000000000000000000 ) ) ;
#874 = CARTESIAN_POINT ( 'NONE',  ( 2.255140518769849223E-14, 49.00000000000000000, 3.499999999999992895 ) ) ;
#875 = CARTESIAN_POINT ( 'NONE',  ( -20.46659425767094120, 21.93593546006592732, 5.128325996195414405 ) ) ;
#876 = CARTESIAN_POINT ( 'NONE',  ( 3.672066530599467971, 34.22247196340288866, 10.58813356411693185 ) ) ;
#877 = DIRECTION ( 'NONE',  ( 1.000000000000000000, 0.000000000000000000, 0.000000000000000000 ) ) ;
#878 = STYLED_ITEM ( 'NONE', ( #1424 ), #2500 ) ;
#879 = DIRECTION ( 'NONE',  ( 0.000000000000000000, -1.000000000000000000, 0.000000000000000000 ) ) ;
#880 = ORIENTED_EDGE ( 'NONE', *, *, #583, .T. ) ;
#881 = ORIENTED_EDGE ( 'NONE', *, *, #3334, .F. ) ;
#882 = ORIENTED_EDGE ( 'NONE', *, *, #3578, .T. ) ;
#883 = VERTEX_POINT ( 'NONE', #433 ) ;
#884 = CARTESIAN_POINT ( 'NONE',  ( 0.000000000000000000, 0.000000000000000000, 20.00000000000000000 ) ) ;
#885 = PRESENTATION_LAYER_ASSIGNMENT (  '', '', ( #2621 ) ) ;
#886 = CIRCLE ( 'NONE', #3466, 5.500000000000000000 ) ;
#887 = FILL_AREA_STYLE ('',( #1690 ) ) ;
#888 = DIRECTION ( 'NONE',  ( 1.000000000000000000, -0.000000000000000000, -0.000000000000000000 ) ) ;
#889 = CARTESIAN_POINT ( 'NONE',  ( 3.889087296526035242, 49.00000000000000000, 5.110912703473999841 ) ) ;
#890 = AXIS2_PLACEMENT_3D ( 'NONE', #718, #3932, #1027 ) ;
#891 = ADVANCED_FACE ( 'NONE', ( #1883 ), #3893, .F. ) ;
#892 = LINE ( 'NONE', #4485, #4501 ) ;
#893 = FACE_BOUND ( 'NONE', #793, .T. ) ;
#894 = DIRECTION ( 'NONE',  ( 0.000000000000000000, 1.000000000000000000, 0.000000000000000000 ) ) ;
#895 = VERTEX_POINT ( 'NONE', #792 ) ;
#896 = ADVANCED_FACE ( 'NONE', ( #1497 ), #83, .T. ) ;
#897 = EDGE_CURVE ( 'NONE', #1997, #4134, #2797, .T. ) ;
#898 = CARTESIAN_POINT ( 'NONE',  ( -3.180741987853693331, 29.83126030492351788, 11.43940974718624837 ) ) ;
#899 = DIRECTION ( 'NONE',  ( -0.000000000000000000, 0.000000000000000000, 1.000000000000000000 ) ) ;
#900 = VECTOR ( 'NONE', #4268, 1000.000000000000000 ) ;
#901 = CARTESIAN_POINT ( 'NONE',  ( 0.000000000000000000, 0.000000000000000000, 19.50000000000000000 ) ) ;
#902 = AXIS2_PLACEMENT_3D ( 'NONE', #2490, #3214, #3962 ) ;
#903 = DIRECTION ( 'NONE',  ( -0.7071067811865487940, -0.7071067811865463515, 0.000000000000000000 ) ) ;
#904 = DIRECTION ( 'NONE',  ( 0.000000000000000000, 0.000000000000000000, 1.000000000000000000 ) ) ;
#905 = CYLINDRICAL_SURFACE ( 'NONE', #367, 1.000000000000000000 ) ;
#906 = VERTEX_POINT ( 'NONE', #3530 ) ;
#907 = VERTEX_POINT ( 'NONE', #276 ) ;
#908 = ORIENTED_EDGE ( 'NONE', *, *, #3418, .F. ) ;
#909 = EDGE_LOOP ( 'NONE', ( #4375, #2617, #4238, #1805 ) ) ;
#910 = CARTESIAN_POINT ( 'NONE',  ( 3.959305739469038251E-15, 30.00000000000000355, 12.99999999999999289 ) ) ;
#911 = DIRECTION ( 'NONE',  ( -0.000000000000000000, -0.000000000000000000, -1.000000000000000000 ) ) ;
#912 = CARTESIAN_POINT ( 'NONE',  ( 3.469446951953614189E-15, 25.00000000000000000, 8.999999999999992895 ) ) ;
#913 = DIRECTION ( 'NONE',  ( 0.000000000000000000, 0.000000000000000000, -1.000000000000000000 ) ) ;
#914 = ADVANCED_FACE ( 'NONE', ( #4637 ), #2820, .F. ) ;
#915 = DIRECTION ( 'NONE',  ( -0.000000000000000000, -0.000000000000000000, -1.000000000000000000 ) ) ;
#916 = EDGE_CURVE ( 'NONE', #22, #310, #1522, .T. ) ;
#917 =( LENGTH_UNIT ( ) NAMED_UNIT ( * ) SI_UNIT ( .MILLI., .METRE. ) );
#918 = CYLINDRICAL_SURFACE ( 'NONE', #4520, 1.749999999999999778 ) ;
#919 = ORIENTED_EDGE ( 'NONE', *, *, #828, .T. ) ;
#920 = APPLICATION_CONTEXT ( 'automotive_design' ) ;
#921 = AXIS2_PLACEMENT_3D ( 'NONE', #2968, #2293, #2676 ) ;
#922 = CARTESIAN_POINT ( 'NONE',  ( -5.409090909090905619, 49.00000000000000000, 9.995859195463930646 ) ) ;
#923 = DIRECTION ( 'NONE',  ( -0.000000000000000000, -1.000000000000000000, -0.000000000000000000 ) ) ;
#924 = EDGE_CURVE ( 'NONE', #816, #2965, #55, .T. ) ;
#925 = EDGE_CURVE ( 'NONE', #1922, #378, #3566, .T. ) ;
#926 = DIRECTION ( 'NONE',  ( 0.000000000000000000, 0.000000000000000000, -1.000000000000000000 ) ) ;
#927 = DIRECTION ( 'NONE',  ( 1.621111868633889227E-15, 1.000000000000000000, 0.000000000000000000 ) ) ;
#928 = PRODUCT_DEFINITION_SHAPE ( 'NONE', 'NONE',  #2893 ) ;
#929 = PRESENTATION_STYLE_ASSIGNMENT (( #2652 ) ) ;
#930 = CARTESIAN_POINT ( 'NONE',  ( -30.00000000000004974, 29.99999999999995737, 8.999999999999992895 ) ) ;
#931 = EDGE_LOOP ( 'NONE', ( #3447, #2373, #34, #4420, #3973, #4198, #492, #4425 ) ) ;
#932 = EDGE_CURVE ( 'NONE', #1142, #3862, #4379, .T. ) ;
#933 = ORIENTED_EDGE ( 'NONE', *, *, #4502, .F. ) ;
#934 = ORIENTED_EDGE ( 'NONE', *, *, #3848, .F. ) ;
#935 = ORIENTED_EDGE ( 'NONE', *, *, #2783, .T. ) ;
#936 = DIRECTION ( 'NONE',  ( 0.000000000000000000, 1.000000000000000000, 0.000000000000000000 ) ) ;
#937 = AXIS2_PLACEMENT_3D ( 'NONE', #2131, #1063, #2405 ) ;
#938 = FACE_OUTER_BOUND ( 'NONE', #842, .T. ) ;
#939 = B_SPLINE_CURVE_WITH_KNOTS ( 'NONE', 3,
 ( #3550, #361, #4320, #3942, #4662, #2626, #1434, #683, #1814, #2127, #1391, #319, #1769, #3219, #4687, #1060, #3265, #13, #1456, #1108, #3645, #2237, #486, #411, #752, #3006, #845, #4435 ),
 .UNSPECIFIED., .F., .F.,
 ( 4, 2, 2, 2, 2, 2, 2, 2, 2, 2, 2, 2, 2, 4 ),
 ( 0.000000000000000000, 0.0003975746136738169344, 0.0007951492273476338688, 0.001590298454695268605, 0.002385447682042902799, 0.002783022295716720655, 0.003180596909390538511, 0.003578171523064356367, 0.003975746136738174223, 0.004373320750411992079, 0.004770895364085809068, 0.005566044591433457790, 0.005963619205107282585, 0.006361193818781106513 ),
 .UNSPECIFIED. ) ;
#940 = FACE_OUTER_BOUND ( 'NONE', #970, .T. ) ;
#941 = VECTOR ( 'NONE', #269, 1000.000000000000000 ) ;
#942 = ORIENTED_EDGE ( 'NONE', *, *, #2058, .F. ) ;
#943 = VECTOR ( 'NONE', #1692, 1000.000000000000000 ) ;
#944 = DIRECTION ( 'NONE',  ( 0.7071067811865487940, -0.7071067811865463515, 0.000000000000000000 ) ) ;
#945 = DIRECTION ( 'NONE',  ( 1.000000000000000000, 0.000000000000000000, 0.000000000000000000 ) ) ;
#946 = CYLINDRICAL_SURFACE ( 'NONE', #2530, 5.000000000000000888 ) ;
#947 = ORIENTED_EDGE ( 'NONE', *, *, #693, .T. ) ;
#948 = CARTESIAN_POINT ( 'NONE',  ( -0.5265545572341292502, 29.99647701088549923, 12.97381592328244082 ) ) ;
#949 = CARTESIAN_POINT ( 'NONE',  ( 3.889087296526035242, 37.00000000000000000, 6.110912703473999841 ) ) ;
#950 = CIRCLE ( 'NONE', #3602, 8.000000000000000000 ) ;
#951 = PLANE ( 'NONE',  #848 ) ;
#952 = CARTESIAN_POINT ( 'NONE',  ( -17.67766952966371719, 17.67766952966366389, 8.999999999999992895 ) ) ;
#953 = DIRECTION ( 'NONE',  ( 0.7071067811865462405, 0.7071067811865487940, 0.000000000000000000 ) ) ;
#954 = VERTEX_POINT ( 'NONE', #1825 ) ;
#955 = AXIS2_PLACEMENT_3D ( 'NONE', #1133, #2645, #3717 ) ;
#956 = VERTEX_POINT ( 'NONE', #1781 ) ;
#957 = ADVANCED_FACE ( 'NONE', ( #3302 ), #1952, .T. ) ;
#958 = ORIENTED_EDGE ( 'NONE', *, *, #4634, .T. ) ;
#959 = CARTESIAN_POINT ( 'NONE',  ( 0.5000000000000000000, 0.8660254037844387076, 19.50000000000000000 ) ) ;
#960 = ADVANCED_FACE ( 'NONE', ( #4674 ), #2853, .T. ) ;
#961 = CYLINDRICAL_SURFACE ( 'NONE', #2888, 5.500000000000000000 ) ;
#962 = AXIS2_PLACEMENT_3D ( 'NONE', #3454, #3122, #3098 ) ;
#963 = B_SPLINE_CURVE_WITH_KNOTS ( 'NONE', 3,
 ( #3619, #2631, #2268, #2675, #1974, #1608, #1899, #876, #2247, #4140, #145, #2313, #4359, #494, #358, #3781, #1585, #165, #2291, #3061, #4516, #1103, #3983, #1809, #11, #1451, #1949, #4094, #3370, #2907 ),
 .UNSPECIFIED., .F., .F.,
 ( 4, 2, 2, 2, 2, 2, 2, 2, 2, 2, 2, 2, 2, 2, 4 ),
 ( 0.006361193818781106513, 0.006758065648931968657, 0.007154937479082830801, 0.007551809309233692945, 0.007948681139384555089, 0.008345552969535416366, 0.008742424799686279377, 0.009536168459987998461, 0.009933040290138858003, 0.01032991212028971928, 0.01112365578059143836, 0.01152052761074228923, 0.01191739944089314357, 0.01231427127104399617, 0.01271114310119484878 ),
 .UNSPECIFIED. ) ;
#964 = FACE_OUTER_BOUND ( 'NONE', #1217, .T. ) ;
#965 = ORIENTED_EDGE ( 'NONE', *, *, #4384, .T. ) ;
#966 = CARTESIAN_POINT ( 'NONE',  ( -8.999999999999969802, 34.74999999999999289, 2.143131898507857451E-16 ) ) ;
#967 =( NAMED_UNIT ( * ) PLANE_ANGLE_UNIT ( ) SI_UNIT ( $, .RADIAN. ) );
#968 = DIRECTION ( 'NONE',  ( 1.000000000000000000, 0.000000000000000000, -0.000000000000000000 ) ) ;
#969 = AXIS2_PLACEMENT_3D ( 'NONE', #3062, #4636, #495 ) ;
#970 = EDGE_LOOP ( 'NONE', ( #3118, #2045, #646, #4146 ) ) ;
#971 = VECTOR ( 'NONE', #2847, 1000.000000000000000 ) ;
#972 = DIRECTION ( 'NONE',  ( 1.000000000000000000, 0.000000000000000000, 0.000000000000000000 ) ) ;
#973 = DIRECTION ( 'NONE',  ( -0.000000000000000000, 1.000000000000000000, -0.000000000000000000 ) ) ;
#974 = EDGE_CURVE ( 'NONE', #127, #2969, #1720, .T. ) ;
#975 = CARTESIAN_POINT ( 'NONE',  ( -0.7500000000000000000, -1.299038105676658450, 18.19999999999999929 ) ) ;
#976 = FACE_OUTER_BOUND ( 'NONE', #2756, .T. ) ;
#977 = CARTESIAN_POINT ( 'NONE',  ( -27.99999999999999645, 0.000000000000000000, 20.00000000000000000 ) ) ;
#978 = CARTESIAN_POINT ( 'NONE',  ( -26.00000000000000000, 1.701696020694461131, 20.00001199999999812 ) ) ;
#979 = ORIENTED_EDGE ( 'NONE', *, *, #4589, .T. ) ;
#980 = ORIENTED_EDGE ( 'NONE', *, *, #281, .F. ) ;
#981 = ORIENTED_EDGE ( 'NONE', *, *, #1897, .T. ) ;
#982 = CIRCLE ( 'NONE', #4392, 1.749999999999999778 ) ;
#983 = LINE ( 'NONE', #4201, #2873 ) ;
#984 = FILL_AREA_STYLE ('',( #1004 ) ) ;
#985 = PRESENTATION_LAYER_ASSIGNMENT (  '', '', ( #606 ) ) ;
#986 = DIRECTION ( 'NONE',  ( 0.000000000000000000, 1.000000000000000000, 0.000000000000000000 ) ) ;
#987 = EDGE_CURVE ( 'NONE', #2090, #3682, #1802, .T. ) ;
#988 = DIRECTION ( 'NONE',  ( 1.000000000000000000, 0.000000000000000000, 0.000000000000000000 ) ) ;
#989 = CIRCLE ( 'NONE', #3032, 4.000000000000000000 ) ;
#990 = DIRECTION ( 'NONE',  ( -0.000000000000000000, -1.000000000000000000, 0.000000000000000000 ) ) ;
#991 = CARTESIAN_POINT ( 'NONE',  ( 3.593167859435787204, 29.78421435497087444, 10.77704851721127177 ) ) ;
#992 = ORIENTED_EDGE ( 'NONE', *, *, #4436, .T. ) ;
#993 = CARTESIAN_POINT ( 'NONE',  ( -1.039771317798496408, 29.98307469845295969, 12.87134967428165666 ) ) ;
#994 = CARTESIAN_POINT ( 'NONE',  ( -27.10000000000000497, -0.5999999999999998668, 19.59999999999999787 ) ) ;
#995 = AXIS2_PLACEMENT_3D ( 'NONE', #2650, #4193, #2333 ) ;
#996 = LINE ( 'NONE', #2062, #248 ) ;
#997 = DIRECTION ( 'NONE',  ( 0.000000000000000000, 1.000000000000000000, 0.000000000000000000 ) ) ;
#998 = CARTESIAN_POINT ( 'NONE',  ( 26.49999999999999645, -0.5000000000000000000, 19.00000000000000000 ) ) ;
#999 = ORIENTED_EDGE ( 'NONE', *, *, #1043, .F. ) ;
#1000 = ORIENTED_EDGE ( 'NONE', *, *, #3421, .F. ) ;
#1001 = DIRECTION ( 'NONE',  ( 0.000000000000000000, 0.000000000000000000, 1.000000000000000000 ) ) ;
#1002 = DIRECTION ( 'NONE',  ( -0.000000000000000000, -1.000000000000000000, -0.000000000000000000 ) ) ;
#1003 = PRESENTATION_STYLE_ASSIGNMENT (( #2485 ) ) ;
#1004 = FILL_AREA_STYLE_COLOUR ( '', #1477 ) ;
#1005 = CARTESIAN_POINT ( 'NONE',  ( -6.741346781237239405, 25.16843286583313954, 20.00001200000000168 ) ) ;
#1006 = CIRCLE ( 'NONE', #3202, 1.500000000000000222 ) ;
#1007 = DIRECTION ( 'NONE',  ( 0.000000000000000000, 0.000000000000000000, 1.000000000000000000 ) ) ;
#1008 = DIRECTION ( 'NONE',  ( 1.000000000000000000, 0.000000000000000000, 0.000000000000000000 ) ) ;
#1009 = CARTESIAN_POINT ( 'NONE',  ( 1.042990544031788813, 29.98297896446152322, 5.129385753419673399 ) ) ;
#1010 = ORIENTED_EDGE ( 'NONE', *, *, #142, .F. ) ;
#1011 = EDGE_CURVE ( 'NONE', #1930, #2608, #4613, .T. ) ;
#1012 = ADVANCED_FACE ( 'NONE', ( #1758, #3611 ), #1380, .T. ) ;
#1013 = DIRECTION ( 'NONE',  ( 0.000000000000000000, 0.000000000000000000, 1.000000000000000000 ) ) ;
#1014 = DIRECTION ( 'NONE',  ( -1.000000000000000000, 0.000000000000000000, 0.000000000000000000 ) ) ;
#1015 =( NAMED_UNIT ( * ) PLANE_ANGLE_UNIT ( ) SI_UNIT ( $, .RADIAN. ) );
#1016 = CARTESIAN_POINT ( 'NONE',  ( 13.02991752792604174, -22.56362157461193263, 20.00001200000000168 ) ) ;
#1017 = CARTESIAN_POINT ( 'NONE',  ( -23.85222316637485562, 18.19536891688241909, 8.738792385868096702 ) ) ;
#1018 = LINE ( 'NONE', #3627, #2450 ) ;
#1019 = CARTESIAN_POINT ( 'NONE',  ( -3.967457472430134580, 34.93422823600056404, 8.474369013652145455 ) ) ;
#1020 = ORIENTED_EDGE ( 'NONE', *, *, #3950, .T. ) ;
#1021 = ORIENTED_EDGE ( 'NONE', *, *, #4190, .F. ) ;
#1022 = CIRCLE ( 'NONE', #1936, 1.000000000000000888 ) ;
#1023 = DIRECTION ( 'NONE',  ( -1.000000000000000000, 0.000000000000000000, 0.000000000000000000 ) ) ;
#1024 = DIRECTION ( 'NONE',  ( 0.000000000000000000, -0.000000000000000000, 1.000000000000000000 ) ) ;
#1025 =( LENGTH_UNIT ( ) NAMED_UNIT ( * ) SI_UNIT ( .MILLI., .METRE. ) );
#1026 = CIRCLE ( 'NONE', #2452, 4.000000000000000000 ) ;
#1027 = DIRECTION ( 'NONE',  ( 0.000000000000000000, 0.000000000000000000, 1.000000000000000000 ) ) ;
#1028 = ORIENTED_EDGE ( 'NONE', *, *, #1435, .F. ) ;
#1029 = CARTESIAN_POINT ( 'NONE',  ( 25.99519186311192342, -0.5000000000000000000, 20.00000000000000000 ) ) ;
#1030 = COLOUR_RGB ( '',0.8941176470588234615, 0.8941176470588234615, 0.8941176470588234615 ) ;
#1031 = CYLINDRICAL_SURFACE ( 'NONE', #3057, 0.5000000000000001110 ) ;
#1032 = CARTESIAN_POINT ( 'NONE',  ( 13.75000000000000178, 36.00000000000000000, 0.000000000000000000 ) ) ;
#1033 = CARTESIAN_POINT ( 'NONE',  ( 3.472993751331377332, 29.79865100271689471, 6.998343904161816731 ) ) ;
#1034 = EDGE_CURVE ( 'NONE', #181, #289, #4312, .T. ) ;
#1035 = EDGE_CURVE ( 'NONE', #2995, #4460, #2546, .T. ) ;
#1036 = FILL_AREA_STYLE ('',( #4273 ) ) ;
#1037 = COLOUR_RGB ( '',0.8941176470588234615, 0.8941176470588234615, 0.8941176470588234615 ) ;
#1038 = AXIS2_PLACEMENT_3D ( 'NONE', #4283, #2088, #691 ) ;
#1039 = CARTESIAN_POINT ( 'NONE',  ( -26.50000000000000355, 0.5000000000000000000, 19.50000000000000000 ) ) ;
#1040 = EDGE_CURVE ( 'NONE', #2780, #85, #1094, .T. ) ;
#1041 = APPLICATION_PROTOCOL_DEFINITION ( 'draft international standard', 'automotive_design', 1998, #3498 ) ;
#1042 = CARTESIAN_POINT ( 'NONE',  ( 19.58805710660147170, -17.18149551509900519, 20.00001200000000523 ) ) ;
#1043 = EDGE_CURVE ( 'NONE', #177, #742, #2922, .T. ) ;
#1044 = CARTESIAN_POINT ( 'NONE',  ( 3.469446951953614189E-15, 43.00000000000000000, 8.999999999999992895 ) ) ;
#1045 = CARTESIAN_POINT ( 'NONE',  ( 0.000000000000000000, 0.000000000000000000, 20.00000000000000000 ) ) ;
#1046 = CARTESIAN_POINT ( 'NONE',  ( -27.10000000000000497, -0.5999999999999998668, 19.00000000000000000 ) ) ;
#1047 = ORIENTED_EDGE ( 'NONE', *, *, #2083, .T. ) ;
#1048 = ORIENTED_EDGE ( 'NONE', *, *, #4587, .T. ) ;
#1049 = CARTESIAN_POINT ( 'NONE',  ( -27.10000000000000497, 0.6000000000000000888, 19.59999999999999787 ) ) ;
#1050 =( NAMED_UNIT ( * ) PLANE_ANGLE_UNIT ( ) SI_UNIT ( $, .RADIAN. ) );
#1051 = CARTESIAN_POINT ( 'NONE',  ( 2.255140518769849223E-14, 34.17157287525380838, 4.499999999999992895 ) ) ;
#1052 = ORIENTED_EDGE ( 'NONE', *, *, #749, .F. ) ;
#1053 = CARTESIAN_POINT ( 'NONE',  ( 0.000000000000000000, 0.000000000000000000, 19.50000000000000000 ) ) ;
#1054 = AXIS2_PLACEMENT_3D ( 'NONE', #725, #2166, #1235 ) ;
#1055 = FACE_OUTER_BOUND ( 'NONE', #1448, .T. ) ;
#1056 = CARTESIAN_POINT ( 'NONE',  ( 3.469446951953614189E-15, 37.00000000000000000, 8.999999999999992895 ) ) ;
#1057 = AXIS2_PLACEMENT_3D ( 'NONE', #767, #357, #430 ) ;
#1058 = DIRECTION ( 'NONE',  ( 1.621111868633889227E-15, 1.000000000000000000, 0.000000000000000000 ) ) ;
#1059 = ADVANCED_FACE ( 'NONE', ( #2531 ), #3958, .T. ) ;
#1060 = CARTESIAN_POINT ( 'NONE',  ( 3.967441838779844687, 31.06580411031222866, 9.525690396061342824 ) ) ;
#1061 = PRODUCT_CONTEXT ( 'NONE', #335, 'mechanical' ) ;
#1062 = CIRCLE ( 'NONE', #4402, 0.5000000000000001110 ) ;
#1063 = DIRECTION ( 'NONE',  ( 0.000000000000000000, 0.000000000000000000, 1.000000000000000000 ) ) ;
#1064 = LINE ( 'NONE', #2194, #2300 ) ;
#1065 = DIRECTION ( 'NONE',  ( 1.000000000000000000, 0.000000000000000000, 0.000000000000000000 ) ) ;
#1066 = EDGE_CURVE ( 'NONE', #3374, #1168, #4164, .T. ) ;
#1067 = CIRCLE ( 'NONE', #692, 0.9999999999999997780 ) ;
#1068 = EDGE_LOOP ( 'NONE', ( #104, #3039, #764, #2252 ) ) ;
#1069 = AXIS2_PLACEMENT_3D ( 'NONE', #4115, #2357, #1284 ) ;
#1070 = EDGE_CURVE ( 'NONE', #4401, #3730, #2816, .T. ) ;
#1071 = ORIENTED_EDGE ( 'NONE', *, *, #2422, .F. ) ;
#1072 = CIRCLE ( 'NONE', #3965, 5.500000000000000000 ) ;
#1073 = EDGE_CURVE ( 'NONE', #3706, #3924, #2200, .T. ) ;
#1074 =( NAMED_UNIT ( * ) PLANE_ANGLE_UNIT ( ) SI_UNIT ( $, .RADIAN. ) );
#1075 = CARTESIAN_POINT ( 'NONE',  ( 5.500000000000003553, 49.00000000000000000, 8.999999999999992895 ) ) ;
#1076 = ORIENTED_EDGE ( 'NONE', *, *, #2773, .F. ) ;
#1077 = CARTESIAN_POINT ( 'NONE',  ( 15.85973458909325728, 20.67279826512042362, 20.00001200000000168 ) ) ;
#1078 = DIRECTION ( 'NONE',  ( 0.000000000000000000, 0.000000000000000000, 1.000000000000000000 ) ) ;
#1079 = CARTESIAN_POINT ( 'NONE',  ( -27.10000000000000497, 0.6000000000000000888, 19.00000000000000000 ) ) ;
#1080 = CARTESIAN_POINT ( 'NONE',  ( 0.000000000000000000, 6.000000000000000000, 20.00000000000000000 ) ) ;
#1081 = AXIS2_PLACEMENT_3D ( 'NONE', #4311, #328, #1423 ) ;
#1082 = CYLINDRICAL_SURFACE ( 'NONE', #4184, 2.000000000000000888 ) ;
#1083 = CLOSED_SHELL ( 'NONE', ( #1845, #4127, #2356, #3065, #4322, #2721, #4192, #3598, #1324, #1603, #2660, #3233 ) ) ;
#1084 = AXIS2_PLACEMENT_3D ( 'NONE', #2427, #2821, #2086 ) ;
#1085 = CARTESIAN_POINT ( 'NONE',  ( 22.42982507849026064, 19.92389804225921068, 12.59566700906149173 ) ) ;
#1086 = CIRCLE ( 'NONE', #3744, 1.000000000000000000 ) ;
#1087 = DIRECTION ( 'NONE',  ( -1.000000000000000000, 0.000000000000000000, 0.000000000000000000 ) ) ;
#1088 = DIRECTION ( 'NONE',  ( -0.000000000000000000, -0.000000000000000000, 1.000000000000000000 ) ) ;
#1089 = LINE ( 'NONE', #2524, #2622 ) ;
#1090 = ORIENTED_EDGE ( 'NONE', *, *, #4551, .T. ) ;
#1091 = ADVANCED_FACE ( 'NONE', ( #398 ), #331, .T. ) ;
#1092 = EDGE_LOOP ( 'NONE', ( #934, #1967, #4570, #1475 ) ) ;
#1093 = PLANE ( 'NONE',  #3890 ) ;
#1094 = LINE ( 'NONE', #4313, #1117 ) ;
#1095 = ORIENTED_EDGE ( 'NONE', *, *, #3106, .F. ) ;
#1096 = CIRCLE ( 'NONE', #3147, 0.7500000000000001110 ) ;
#1097 = EDGE_LOOP ( 'NONE', ( #4260, #810, #1357, #2559 ) ) ;
#1098 = VERTEX_POINT ( 'NONE', #1901 ) ;
#1099 = ADVANCED_FACE ( 'NONE', ( #4046 ), #1518, .T. ) ;
#1100 = ADVANCED_FACE ( 'NONE', ( #1926 ), #4450, .F. ) ;
#1101 = DIRECTION ( 'NONE',  ( 0.000000000000000000, 0.000000000000000000, 1.000000000000000000 ) ) ;
#1102 = AXIS2_PLACEMENT_3D ( 'NONE', #3571, #2494, #4338 ) ;
#1103 = CARTESIAN_POINT ( 'NONE',  ( 3.706735793540077761, 34.32176079584164086, 7.493470964888216734 ) ) ;
#1104 = DIRECTION ( 'NONE',  ( -0.000000000000000000, -0.000000000000000000, -1.000000000000000000 ) ) ;
#1105 = EDGE_LOOP ( 'NONE', ( #2628, #1291, #1658, #3274 ) ) ;
#1106 = AXIS2_PLACEMENT_3D ( 'NONE', #3743, #1553, #62 ) ;
#1107 = AXIS2_PLACEMENT_3D ( 'NONE', #4548, #3049, #2713 ) ;
#1108 = CARTESIAN_POINT ( 'NONE',  ( 3.809422024637068471, 31.41382050535269954, 10.22508852591141348 ) ) ;
#1109 = SHAPE_DEFINITION_REPRESENTATION ( #3051, #1408 ) ;
#1110 = EDGE_CURVE ( 'NONE', #3335, #4618, #1587, .T. ) ;
#1111 = COLOUR_RGB ( '',0.8941176470588234615, 0.8941176470588234615, 0.8941176470588234615 ) ;
#1112 = AXIS2_PLACEMENT_3D ( 'NONE', #4369, #3581, #325 ) ;
#1113 = DIRECTION ( 'NONE',  ( 1.000000000000000000, 0.000000000000000000, 0.000000000000000000 ) ) ;
#1114 = CYLINDRICAL_SURFACE ( 'NONE', #4514, 26.00000000000000711 ) ;
#1115 = DIRECTION ( 'NONE',  ( 0.000000000000000000, 0.000000000000000000, -1.000000000000000000 ) ) ;
#1116 = PRODUCT_DEFINITION_FORMATION_WITH_SPECIFIED_SOURCE ( 'ANY', '', #2031, .NOT_KNOWN. ) ;
#1117 = VECTOR ( 'NONE', #2486, 1000.000000000000000 ) ;
#1118 = ORIENTED_EDGE ( 'NONE', *, *, #2395, .T. ) ;
#1119 = ORIENTED_EDGE ( 'NONE', *, *, #3787, .F. ) ;
#1120 = CARTESIAN_POINT ( 'NONE',  ( -3.472185852622982516, 32.73050154287725633, 7.013837769849707193 ) ) ;
#1121 = DIRECTION ( 'NONE',  ( 0.7071067811865456854, 8.659560562354910671E-17, -0.7071067811865493491 ) ) ;
#1122 = ORIENTED_EDGE ( 'NONE', *, *, #1453, .F. ) ;
#1123 = ORIENTED_EDGE ( 'NONE', *, *, #514, .F. ) ;
#1124 = ORIENTED_EDGE ( 'NONE', *, *, #2983, .F. ) ;
#1125 = CARTESIAN_POINT ( 'NONE',  ( 25.99307600111999150, 0.6000000000000000888, 20.00001200000000168 ) ) ;
#1126 = CARTESIAN_POINT ( 'NONE',  ( 0.7500000000000001110, 1.299038105676658450, 17.69999999999999929 ) ) ;
#1127 = DIRECTION ( 'NONE',  ( 0.000000000000000000, 0.000000000000000000, 1.000000000000000000 ) ) ;
#1128 = CARTESIAN_POINT ( 'NONE',  ( -22.56362157461193618, -13.02991752792603641, 20.00001200000000168 ) ) ;
#1129 = EDGE_CURVE ( 'NONE', #1185, #1877, #4475, .T. ) ;
#1130 = ORIENTED_EDGE ( 'NONE', *, *, #4580, .F. ) ;
#1131 = EDGE_CURVE ( 'NONE', #3723, #2120, #2345, .T. ) ;
#1132 = DIRECTION ( 'NONE',  ( -0.000000000000000000, -0.000000000000000000, -1.000000000000000000 ) ) ;
#1133 = CARTESIAN_POINT ( 'NONE',  ( -8.999999999999998224, 36.00000000000000711, 0.000000000000000000 ) ) ;
#1134 = PRODUCT_CONTEXT ( 'NONE', #590, 'mechanical' ) ;
#1135 = AXIS2_PLACEMENT_3D ( 'NONE', #3491, #236, #3136 ) ;
#1136 = CIRCLE ( 'NONE', #2119, 5.500000000000000000 ) ;
#1137 = CARTESIAN_POINT ( 'NONE',  ( 18.84534098761077914, 23.34254382248196791, 6.559627254860783019 ) ) ;
#1138 = CARTESIAN_POINT ( 'NONE',  ( 0.000000000000000000, 0.000000000000000000, 19.00000000000000000 ) ) ;
#1139 = VECTOR ( 'NONE', #3148, 1000.000000000000000 ) ;
#1140 = CARTESIAN_POINT ( 'NONE',  ( 0.000000000000000000, 0.000000000000000000, 16.00000000000000000 ) ) ;
#1141 = ORIENTED_EDGE ( 'NONE', *, *, #2112, .F. ) ;
#1142 = VERTEX_POINT ( 'NONE', #1213 ) ;
#1143 = CARTESIAN_POINT ( 'NONE',  ( 0.000000000000000000, 0.000000000000000000, 17.00000000000000000 ) ) ;
#1144 =( NAMED_UNIT ( * ) PLANE_ANGLE_UNIT ( ) SI_UNIT ( $, .RADIAN. ) );
#1145 = DIRECTION ( 'NONE',  ( 0.000000000000000000, 1.000000000000000000, 0.000000000000000000 ) ) ;
#1146 = VERTEX_POINT ( 'NONE', #3349 ) ;
#1147 = ORIENTED_EDGE ( 'NONE', *, *, #45, .T. ) ;
#1148 = VERTEX_POINT ( 'NONE', #3751 ) ;
#1149 = LINE ( 'NONE', #1125, #4279 ) ;
#1150 = TOROIDAL_SURFACE ( 'NONE', #1749, 3.000000000000002665, 1.749999999999999778 ) ;
#1151 = CARTESIAN_POINT ( 'NONE',  ( -19.75109744359749797, 22.58188871325890901, 12.47298490618377897 ) ) ;
#1152 = CARTESIAN_POINT ( 'NONE',  ( -17.18149551509900519, -19.58805710660146104, 20.00001200000000523 ) ) ;
#1153 = ORIENTED_EDGE ( 'NONE', *, *, #2783, .F. ) ;
#1154 = DIRECTION ( 'NONE',  ( 0.7071067811865462405, 0.7071067811865487940, 0.000000000000000000 ) ) ;
#1155 = ADVANCED_FACE ( 'NONE', ( #1512 ), #3400, .T. ) ;
#1156 = EDGE_CURVE ( 'NONE', #2707, #1507, #2249, .T. ) ;
#1157 = AXIS2_PLACEMENT_3D ( 'NONE', #3694, #1863, #2600 ) ;
#1158 = CARTESIAN_POINT ( 'NONE',  ( 18.97448886297823378, 23.23798364781081816, 6.357861838490106443 ) ) ;
#1159 = CARTESIAN_POINT ( 'NONE',  ( -1.036406108997123487, 29.98318460927812268, 5.127803451112008304 ) ) ;
#1160 = CARTESIAN_POINT ( 'NONE',  ( -3.900351855253532118, 34.79297846328978494, 9.895868398202676275 ) ) ;
#1161 = VERTEX_POINT ( 'NONE', #809 ) ;
#1162 = ORIENTED_EDGE ( 'NONE', *, *, #4064, .T. ) ;
#1163 = CARTESIAN_POINT ( 'NONE',  ( -3.900821110013151127, 31.20601586925484128, 9.893616917921782772 ) ) ;
#1164 =( NAMED_UNIT ( * ) PLANE_ANGLE_UNIT ( ) SI_UNIT ( $, .RADIAN. ) );
#1165 = CARTESIAN_POINT ( 'NONE',  ( 5.409090909090912724, 49.00000000000000000, 9.995859195463930646 ) ) ;
#1166 = ORIENTED_EDGE ( 'NONE', *, *, #4352, .T. ) ;
#1167 = ORIENTED_EDGE ( 'NONE', *, *, #2110, .T. ) ;
#1168 = VERTEX_POINT ( 'NONE', #1165 ) ;
#1169 = UNCERTAINTY_MEASURE_WITH_UNIT (LENGTH_MEASURE( 1.000000000000000082E-05 ), #3518, 'distance_accuracy_value', 'NONE');
#1170 = LINE ( 'NONE', #4456, #750 ) ;
#1171 = CARTESIAN_POINT ( 'NONE',  ( -12.00000000000000178, 36.00000000000001421, 0.000000000000000000 ) ) ;
#1172 = CARTESIAN_POINT ( 'NONE',  ( 3.959305671612554781E-15, 41.00000000000000000, 12.99999999999999289 ) ) ;
#1173 = ORIENTED_EDGE ( 'NONE', *, *, #1731, .F. ) ;
#1174 = AXIS2_PLACEMENT_3D ( 'NONE', #4112, #1891, #2647 ) ;
#1175 = DIRECTION ( 'NONE',  ( -0.000000000000000000, -0.000000000000000000, -1.000000000000000000 ) ) ;
#1176 = DIRECTION ( 'NONE',  ( 0.000000000000000000, 0.000000000000000000, 1.000000000000000000 ) ) ;
#1177 = EDGE_CURVE ( 'NONE', #3258, #4401, #3344, .T. ) ;
#1178 = AXIS2_PLACEMENT_3D ( 'NONE', #175, #3762, #2028 ) ;
#1179 = FACE_OUTER_BOUND ( 'NONE', #126, .T. ) ;
#1180 = DIRECTION ( 'NONE',  ( 1.000000000000000000, 0.000000000000000000, -0.000000000000000000 ) ) ;
#1181 = ADVANCED_FACE ( 'NONE', ( #474 ), #423, .T. ) ;
#1182 = LINE ( 'NONE', #1921, #2934 ) ;
#1183 = ORIENTED_EDGE ( 'NONE', *, *, #3553, .T. ) ;
#1184 =( GEOMETRIC_REPRESENTATION_CONTEXT ( 3 ) GLOBAL_UNCERTAINTY_ASSIGNED_CONTEXT ( ( #1246 ) ) GLOBAL_UNIT_ASSIGNED_CONTEXT ( ( #1619, #2368, #2391 ) ) REPRESENTATION_CONTEXT ( 'NONE', 'WORKASPACE' ) );
#1185 = VERTEX_POINT ( 'NONE', #3678 ) ;
#1186 = CARTESIAN_POINT ( 'NONE',  ( -3.993355759804213090, 31.01319048188283034, 8.734987511292612083 ) ) ;
#1187 = DIRECTION ( 'NONE',  ( 0.000000000000000000, 0.000000000000000000, 1.000000000000000000 ) ) ;
#1188 = SHAPE_REPRESENTATION_RELATIONSHIP ( 'NONE' , 'NONE' ,  #1892, #4552 ) ;
#1189 = CARTESIAN_POINT ( 'NONE',  ( 23.83633674995677509, 18.21624787168408588, 8.475268202211099222 ) ) ;
#1190 = AXIS2_PLACEMENT_3D ( 'NONE', #2109, #1819, #1396 ) ;
#1191 = CARTESIAN_POINT ( 'NONE',  ( 3.469446951953614189E-15, 25.00000000000000000, 4.999999999999992006 ) ) ;
#1192 = VERTEX_POINT ( 'NONE', #854 ) ;
#1193 = ORIENTED_EDGE ( 'NONE', *, *, #283, .F. ) ;
#1194 = EDGE_LOOP ( 'NONE', ( #1868, #3653, #4355, #573, #2187, #3019, #2155, #2363, #675, #1469, #528, #3426, #2410, #1223, #1903, #551, #1462, #3424, #3203 ) ) ;
#1195 = VERTEX_POINT ( 'NONE', #74 ) ;
#1196 = CARTESIAN_POINT ( 'NONE',  ( 5.409090909090912724, 43.00000000000000000, 8.004140804536053366 ) ) ;
#1197 = CARTESIAN_POINT ( 'NONE',  ( -30.00000000000000355, 0.000000000000000000, 17.99999999999998579 ) ) ;
#1198 = LINE ( 'NONE', #3735, #3004 ) ;
#1199 = VERTEX_POINT ( 'NONE', #4495 ) ;
#1200 = DIRECTION ( 'NONE',  ( 0.000000000000000000, 0.000000000000000000, 1.000000000000000000 ) ) ;
#1201 = CARTESIAN_POINT ( 'NONE',  ( -0.5000000000000001110, 0.000000000000000000, 20.00000000000000000 ) ) ;
#1202 = AXIS2_PLACEMENT_3D ( 'NONE', #4076, #80, #3046 ) ;
#1203 = ADVANCED_BREP_SHAPE_REPRESENTATION ( '', ( #1412, #2928 ), #3769 ) ;
#1204 = CARTESIAN_POINT ( 'NONE',  ( 0.000000000000000000, 0.000000000000000000, 17.69999999999999929 ) ) ;
#1205 = AXIS2_PLACEMENT_3D ( 'NONE', #384, #4363, #1860 ) ;
#1206 = FACE_OUTER_BOUND ( 'NONE', #2386, .T. ) ;
#1207 = ORIENTED_EDGE ( 'NONE', *, *, #687, .F. ) ;
#1208 = AXIS2_PLACEMENT_3D ( 'NONE', #1938, #1277, #945 ) ;
#1209 = DIRECTION ( 'NONE',  ( 1.000000000000000000, 0.000000000000000000, 0.000000000000000000 ) ) ;
#1210 = CARTESIAN_POINT ( 'NONE',  ( 18.19536891688249369, 23.85222316637479523, 8.999999999999992895 ) ) ;
#1211 = ADVANCED_FACE ( 'NONE', ( #1238 ), #1489, .T. ) ;
#1212 =( NAMED_UNIT ( * ) SI_UNIT ( $, .STERADIAN. ) SOLID_ANGLE_UNIT ( ) );
#1213 = CARTESIAN_POINT ( 'NONE',  ( 3.469446951953614189E-15, 41.00000000000000000, 12.99999999999999467 ) ) ;
#1214 = ORIENTED_EDGE ( 'NONE', *, *, #866, .T. ) ;
#1215 = ADVANCED_FACE ( 'NONE', ( #4071 ), #101, .F. ) ;
#1216 = ADVANCED_FACE ( 'NONE', ( #3782 ), #2633, .T. ) ;
#1217 = EDGE_LOOP ( 'NONE', ( #1166, #783, #21, #1124 ) ) ;
#1218 = ORIENTED_EDGE ( 'NONE', *, *, #4706, .F. ) ;
#1219 = EDGE_LOOP ( 'NONE', ( #537, #3228, #4593, #1147 ) ) ;
#1220 = CARTESIAN_POINT ( 'NONE',  ( 3.469446951953614189E-15, 37.00000000000000000, 8.999999999999992895 ) ) ;
#1221 = DIRECTION ( 'NONE',  ( 0.000000000000000000, 1.000000000000000000, 0.000000000000000000 ) ) ;
#1222 = DIRECTION ( 'NONE',  ( 0.000000000000000000, 0.000000000000000000, 1.000000000000000000 ) ) ;
#1223 = ORIENTED_EDGE ( 'NONE', *, *, #1066, .F. ) ;
#1224 = CARTESIAN_POINT ( 'NONE',  ( 3.469446951953614189E-15, 30.00000000000000355, 4.999999999999992006 ) ) ;
#1225 = FACE_OUTER_BOUND ( 'NONE', #1963, .T. ) ;
#1226 = CARTESIAN_POINT ( 'NONE',  ( 0.7500000000000001110, 9.184850993605150903E-17, 17.69999999999999929 ) ) ;
#1227 = ITEM_DEFINED_TRANSFORMATION ( 'NONE', 'NONE', #3615,  #2928 ) ;
#1228 = B_SPLINE_CURVE_WITH_KNOTS ( 'NONE', 3,
 ( #3649, #17, #1189, #2549, #4014, #388, #2215, #3668, #92, #2940, #4061, #1890, #414, #3269, #2985, #64, #2962, #4390, #1458, #3291, #4416, #2623, #3340, #2913, #1795, #1158, #1137, #40, #1482, #4438, #1436, #2890, #4087, #822 ),
 .UNSPECIFIED., .F., .F.,
 ( 4, 2, 2, 2, 2, 2, 2, 2, 2, 2, 2, 2, 2, 2, 2, 2, 4 ),
 ( 0.000000000000000000, 0.0007824845743203473133, 0.001564969148640694627, 0.002347453722961044108, 0.003129938297281393590, 0.003912422871601742638, 0.004694907445922092554, 0.005477392020242441602, 0.006259876594562790650, 0.007042361168883141433, 0.007824845743203490481, 0.008607330317523840396, 0.009389814891844192046, 0.01017229946616454196, 0.01095478404048489014, 0.01173726861480523832, 0.01251975318912558477 ),
 .UNSPECIFIED. ) ;
#1229 = PRODUCT ( 'MAS-171', 'MAS-171', '', ( #3601 ) ) ;
#1230 = CARTESIAN_POINT ( 'NONE',  ( 3.469446951953614189E-15, 33.00000000000000000, 8.999999999999992895 ) ) ;
#1231 = CARTESIAN_POINT ( 'NONE',  ( -3.501320667853359048, 33.52543631340415686, 10.93433813232664242 ) ) ;
#1232 = VECTOR ( 'NONE', #2851, 1000.000000000000000 ) ;
#1233 = VECTOR ( 'NONE', #1200, 1000.000000000000000 ) ;
#1234 = DIRECTION ( 'NONE',  ( 0.000000000000000000, 0.000000000000000000, 1.000000000000000000 ) ) ;
#1235 = DIRECTION ( 'NONE',  ( 0.000000000000000000, 0.000000000000000000, 1.000000000000000000 ) ) ;
#1236 = VECTOR ( 'NONE', #2396, 1000.000000000000000 ) ;
#1237 =( NAMED_UNIT ( * ) SI_UNIT ( $, .STERADIAN. ) SOLID_ANGLE_UNIT ( ) );
#1238 = FACE_OUTER_BOUND ( 'NONE', #2957, .T. ) ;
#1239 = VERTEX_POINT ( 'NONE', #1191 ) ;
#1240 = EDGE_CURVE ( 'NONE', #3697, #2686, #1072, .T. ) ;
#1241 = ORIENTED_EDGE ( 'NONE', *, *, #1971, .F. ) ;
#1242 = ORIENTED_EDGE ( 'NONE', *, *, #1620, .T. ) ;
#1243 = EDGE_LOOP ( 'NONE', ( #4067, #570, #933, #1367 ) ) ;
#1244 = DIRECTION ( 'NONE',  ( 0.000000000000000000, -0.000000000000000000, 1.000000000000000000 ) ) ;
#1245 = DIRECTION ( 'NONE',  ( 1.000000000000000000, -0.000000000000000000, -0.000000000000000000 ) ) ;
#1246 = UNCERTAINTY_MEASURE_WITH_UNIT (LENGTH_MEASURE( 1.000000000000000082E-05 ), #1619, 'distance_accuracy_value', 'NONE');
#1247 = SURFACE_STYLE_USAGE ( .BOTH. , #1594 ) ;
#1248 = DIRECTION ( 'NONE',  ( 0.000000000000000000, 0.000000000000000000, -1.000000000000000000 ) ) ;
#1249 = EDGE_CURVE ( 'NONE', #3723, #4511, #4529, .T. ) ;
#1250 = EDGE_CURVE ( 'NONE', #418, #102, #3047, .T. ) ;
#1251 = DIRECTION ( 'NONE',  ( -0.000000000000000000, -1.000000000000000000, -0.000000000000000000 ) ) ;
#1252 = CARTESIAN_POINT ( 'NONE',  ( -13.75000000000000178, 44.99999999999999289, 0.000000000000000000 ) ) ;
#1253 = PLANE ( 'NONE',  #1884 ) ;
#1254 = DIRECTION ( 'NONE',  ( 0.000000000000000000, 1.000000000000000000, 0.000000000000000000 ) ) ;
#1255 = ORIENTED_EDGE ( 'NONE', *, *, #4587, .F. ) ;
#1256 = VECTOR ( 'NONE', #4088, 1000.000000000000000 ) ;
#1257 = AXIS2_PLACEMENT_3D ( 'NONE', #586, #2305, #3768 ) ;
#1258 = LINE ( 'NONE', #2696, #2081 ) ;
#1259 = DIRECTION ( 'NONE',  ( 0.000000000000000000, 0.000000000000000000, 1.000000000000000000 ) ) ;
#1260 = EDGE_CURVE ( 'NONE', #883, #4187, #1640, .T. ) ;
#1261 = AXIS2_PLACEMENT_3D ( 'NONE', #2615, #3685, #2908 ) ;
#1262 = CARTESIAN_POINT ( 'NONE',  ( -19.26183863435818822, 23.00034469605611775, 5.986743120287543185 ) ) ;
#1263 = LINE ( 'NONE', #235, #1850 ) ;
#1264 = EDGE_CURVE ( 'NONE', #468, #4108, #2711, .T. ) ;
#1265 = DIRECTION ( 'NONE',  ( 1.000000000000000000, 0.000000000000000000, 0.000000000000000000 ) ) ;
#1266 = CARTESIAN_POINT ( 'NONE',  ( 25.99307600111999150, 0.5999999999999998668, 19.59999999999999787 ) ) ;
#1267 = EDGE_LOOP ( 'NONE', ( #4285, #6, #743, #3830 ) ) ;
#1268 = ORIENTED_EDGE ( 'NONE', *, *, #2581, .T. ) ;
#1269 = ORIENTED_EDGE ( 'NONE', *, *, #2002, .F. ) ;
#1270 = VERTEX_POINT ( 'NONE', #4177 ) ;
#1271 = CARTESIAN_POINT ( 'NONE',  ( 20.50609665440990526, 14.84924240491746517, 8.999999999999992895 ) ) ;
#1272 =( LENGTH_UNIT ( ) NAMED_UNIT ( * ) SI_UNIT ( .MILLI., .METRE. ) );
#1273 = VECTOR ( 'NONE', #3225, 1000.000000000000000 ) ;
#1274 = ORIENTED_EDGE ( 'NONE', *, *, #2139, .F. ) ;
#1275 = ADVANCED_FACE ( 'NONE', ( #3542 ), #2875, .F. ) ;
#1276 = FACE_OUTER_BOUND ( 'NONE', #1397, .T. ) ;
#1277 = DIRECTION ( 'NONE',  ( 5.782411586589374402E-16, -1.000000000000000000, 0.000000000000000000 ) ) ;
#1278 = DIRECTION ( 'NONE',  ( -0.000000000000000000, -1.000000000000000000, -0.000000000000000000 ) ) ;
#1279 = VERTEX_POINT ( 'NONE', #4525 ) ;
#1280 = ADVANCED_FACE ( 'NONE', ( #3860 ), #4649, .T. ) ;
#1281 = CARTESIAN_POINT ( 'NONE',  ( 18.29783893517735294, 23.77376218378621431, 10.03754308049874133 ) ) ;
#1282 = DIRECTION ( 'NONE',  ( 0.000000000000000000, 1.000000000000000000, 0.000000000000000000 ) ) ;
#1283 = VECTOR ( 'NONE', #1924, 1000.000000000000000 ) ;
#1284 = DIRECTION ( 'NONE',  ( -1.000000000000000000, 0.000000000000000000, 0.000000000000000000 ) ) ;
#1285 = VECTOR ( 'NONE', #336, 1000.000000000000000 ) ;
#1286 = CARTESIAN_POINT ( 'NONE',  ( 12.00000000000000178, 36.00000000000000000, 0.000000000000000000 ) ) ;
#1287 = DIRECTION ( 'NONE',  ( 0.000000000000000000, 0.000000000000000000, 1.000000000000000000 ) ) ;
#1288 = CARTESIAN_POINT ( 'NONE',  ( -17.18149551509903361, 19.58805710660143973, 20.00001200000000168 ) ) ;
#1289 = ORIENTED_EDGE ( 'NONE', *, *, #4086, .T. ) ;
#1290 = VERTEX_POINT ( 'NONE', #3070 ) ;
#1291 = ORIENTED_EDGE ( 'NONE', *, *, #1386, .T. ) ;
#1292 = CIRCLE ( 'NONE', #3178, 26.00000000000000355 ) ;
#1293 = ORIENTED_EDGE ( 'NONE', *, *, #4352, .F. ) ;
#1294 = CIRCLE ( 'NONE', #3029, 1.000000000000000888 ) ;
#1295 = LINE ( 'NONE', #3165, #2483 ) ;
#1296 = DIRECTION ( 'NONE',  ( -0.000000000000000000, -0.000000000000000000, -1.000000000000000000 ) ) ;
#1297 = SURFACE_STYLE_FILL_AREA ( #1595 ) ;
#1298 = AXIS2_PLACEMENT_3D ( 'NONE', #3596, #3193, #1008 ) ;
#1299 = EDGE_LOOP ( 'NONE', ( #1806, #4350, #399, #3813 ) ) ;
#1300 = DIRECTION ( 'NONE',  ( -1.000000000000000000, 0.000000000000000000, 0.000000000000000000 ) ) ;
#1301 = LINE ( 'NONE', #4557, #2188 ) ;
#1302 = DIRECTION ( 'NONE',  ( 0.7071067811865392461, 0.000000000000000000, 0.7071067811865557884 ) ) ;
#1303 = ORIENTED_EDGE ( 'NONE', *, *, #1916, .T. ) ;
#1304 = AXIS2_PLACEMENT_3D ( 'NONE', #4399, #879, #1873 ) ;
#1305 = CARTESIAN_POINT ( 'NONE',  ( 18.19536891688249014, 23.85222316637479523, 9.261144538644668245 ) ) ;
#1306 = EDGE_CURVE ( 'NONE', #715, #1870, #196, .T. ) ;
#1307 = CARTESIAN_POINT ( 'NONE',  ( 0.000000000000000000, 6.000000000000000000, 19.50000000000000000 ) ) ;
#1308 = EDGE_CURVE ( 'NONE', #2854, #305, #4148, .T. ) ;
#1309 = CARTESIAN_POINT ( 'NONE',  ( -18.19536891688249014, 23.85222316637479878, 8.735393166554770161 ) ) ;
#1310 = CARTESIAN_POINT ( 'NONE',  ( 0.000000000000000000, 0.000000000000000000, 19.50000000000000000 ) ) ;
#1311 = AXIS2_PLACEMENT_3D ( 'NONE', #4515, #1234, #143 ) ;
#1312 = CYLINDRICAL_SURFACE ( 'NONE', #4566, 3.999999999999998224 ) ;
#1313 = ORIENTED_EDGE ( 'NONE', *, *, #3981, .T. ) ;
#1314 = ORIENTED_EDGE ( 'NONE', *, *, #23, .T. ) ;
#1315 = VERTEX_POINT ( 'NONE', #3475 ) ;
#1316 = CARTESIAN_POINT ( 'NONE',  ( 3.469446951953614189E-15, 34.00000000000000000, 12.99999999999999467 ) ) ;
#1317 = VECTOR ( 'NONE', #913, 1000.000000000000000 ) ;
#1318 = VECTOR ( 'NONE', #137, 1000.000000000000000 ) ;
#1319 = PRESENTATION_STYLE_ASSIGNMENT (( #3835 ) ) ;
#1320 = SURFACE_STYLE_USAGE ( .BOTH. , #3761 ) ;
#1321 = CARTESIAN_POINT ( 'NONE',  ( 3.959305671612554781E-15, 25.00000000000000000, 12.99999999999999289 ) ) ;
#1322 = CARTESIAN_POINT ( 'NONE',  ( -3.889087296526001047, 49.00000000000000000, 5.110912703473974084 ) ) ;
#1323 = DIRECTION ( 'NONE',  ( 0.000000000000000000, 0.000000000000000000, 1.000000000000000000 ) ) ;
#1324 = ADVANCED_FACE ( 'NONE', ( #3097 ), #1150, .T. ) ;
#1325 = FACE_OUTER_BOUND ( 'NONE', #2294, .T. ) ;
#1326 = LINE ( 'NONE', #2372, #1627 ) ;
#1327 = ORIENTED_EDGE ( 'NONE', *, *, #1910, .T. ) ;
#1328 = DIRECTION ( 'NONE',  ( 0.000000000000000000, 0.000000000000000000, 1.000000000000000000 ) ) ;
#1329 = MANIFOLD_SOLID_BREP ( 'Fillet1', #2747 ) ;
#1330 = CARTESIAN_POINT ( 'NONE',  ( 21.39823644064421160, 21.02820489033393159, 13.00018275065233020 ) ) ;
#1331 = DIRECTION ( 'NONE',  ( 1.000000000000000000, 0.000000000000000000, 0.000000000000000000 ) ) ;
#1332 = CARTESIAN_POINT ( 'NONE',  ( 26.49999999999999645, -0.5000000000000000000, 19.50000000000000000 ) ) ;
#1333 = CARTESIAN_POINT ( 'NONE',  ( 30.00000000000005684, 29.99999999999995026, 8.999999999999992895 ) ) ;
#1334 = CARTESIAN_POINT ( 'NONE',  ( -20.67279826512042717, 15.85973458909326084, 20.00001200000000168 ) ) ;
#1335 = PRODUCT_RELATED_PRODUCT_CATEGORY ( 'part', '', ( #1229 ) ) ;
#1336 = VERTEX_POINT ( 'NONE', #1689 ) ;
#1337 = AXIS2_PLACEMENT_3D ( 'NONE', #3194, #2076, #2167 ) ;
#1338 = ORIENTED_EDGE ( 'NONE', *, *, #4058, .T. ) ;
#1339 = VERTEX_POINT ( 'NONE', #504 ) ;
#1340 = CARTESIAN_POINT ( 'NONE',  ( 3.469446951953614189E-15, 25.00000000000000000, 8.999999999999992895 ) ) ;
#1341 = DIRECTION ( 'NONE',  ( -0.000000000000000000, -1.000000000000000000, -0.000000000000000000 ) ) ;
#1342 = VECTOR ( 'NONE', #3381, 1000.000000000000000 ) ;
#1343 = PLANE ( 'NONE',  #4188 ) ;
#1344 = UNCERTAINTY_MEASURE_WITH_UNIT (LENGTH_MEASURE( 1.000000000000000082E-05 ), #1272, 'distance_accuracy_value', 'NONE');
#1345 = CIRCLE ( 'NONE', #1947, 5.000000000000000888 ) ;
#1346 = CARTESIAN_POINT ( 'NONE',  ( 25.99519186311192342, 0.5000000000000000000, 20.00000000000000000 ) ) ;
#1347 = DIRECTION ( 'NONE',  ( 1.982541115402063335E-15, 1.000000000000000000, 0.000000000000000000 ) ) ;
#1348 = CARTESIAN_POINT ( 'NONE',  ( 3.469446951953614189E-15, 30.00000000000000355, 4.999999999999992006 ) ) ;
#1349 = PRODUCT_DEFINITION_FORMATION_WITH_SPECIFIED_SOURCE ( 'ANY', '', #507, .NOT_KNOWN. ) ;
#1350 = ORIENTED_EDGE ( 'NONE', *, *, #4588, .F. ) ;
#1351 = VECTOR ( 'NONE', #3175, 1000.000000000000000 ) ;
#1352 = CARTESIAN_POINT ( 'NONE',  ( 3.469446951953614189E-15, 49.00000000000000000, 8.999999999999992895 ) ) ;
#1353 = CARTESIAN_POINT ( 'NONE',  ( 18.97463723504673538, 23.23784379901355024, 11.64206388705991557 ) ) ;
#1354 = DIRECTION ( 'NONE',  ( 0.000000000000000000, 0.000000000000000000, 1.000000000000000000 ) ) ;
#1355 = CARTESIAN_POINT ( 'NONE',  ( 0.000000000000000000, 0.000000000000000000, 19.50000000000000000 ) ) ;
#1356 = FACE_OUTER_BOUND ( 'NONE', #3043, .T. ) ;
#1357 = ORIENTED_EDGE ( 'NONE', *, *, #3888, .T. ) ;
#1358 = ORIENTED_EDGE ( 'NONE', *, *, #4137, .F. ) ;
#1359 = AXIS2_PLACEMENT_3D ( 'NONE', #195, #2782, #1377 ) ;
#1360 = DIRECTION ( 'NONE',  ( 0.000000000000000000, 0.000000000000000000, -1.000000000000000000 ) ) ;
#1361 = ADVANCED_FACE ( 'NONE', ( #3429 ), #3142, .F. ) ;
#1362 = ADVANCED_FACE ( 'NONE', ( #938 ), #961, .T. ) ;
#1363 = CARTESIAN_POINT ( 'NONE',  ( 3.959305671612554781E-15, 30.00000000000000355, 12.99999999999999289 ) ) ;
#1364 = CARTESIAN_POINT ( 'NONE',  ( 3.469446951953614189E-15, 49.00000000000000000, 8.999999999999992895 ) ) ;
#1365 = FACE_OUTER_BOUND ( 'NONE', #1708, .T. ) ;
#1366 = CARTESIAN_POINT ( 'NONE',  ( 26.49999999999999645, -0.5000000000000000000, 19.50000000000000000 ) ) ;
#1367 = ORIENTED_EDGE ( 'NONE', *, *, #4282, .T. ) ;
#1368 = SURFACE_STYLE_FILL_AREA ( #1036 ) ;
#1369 = DIRECTION ( 'NONE',  ( -0.000000000000000000, -1.000000000000000000, 0.000000000000000000 ) ) ;
#1370 = DIRECTION ( 'NONE',  ( 0.000000000000000000, 0.000000000000000000, 1.000000000000000000 ) ) ;
#1371 = CARTESIAN_POINT ( 'NONE',  ( -26.50000000000000355, -0.5000000000000000000, 19.50000000000000000 ) ) ;
#1372 = LINE ( 'NONE', #3247, #2978 ) ;
#1373 = FACE_OUTER_BOUND ( 'NONE', #857, .T. ) ;
#1374 = CARTESIAN_POINT ( 'NONE',  ( -3.876963039844159020, 34.74320821126782732, 7.985516166298877394 ) ) ;
#1375 = VERTEX_POINT ( 'NONE', #3406 ) ;
#1376 = ORIENTED_EDGE ( 'NONE', *, *, #4469, .T. ) ;
#1377 = DIRECTION ( 'NONE',  ( 1.000000000000000000, 0.000000000000000000, 0.000000000000000000 ) ) ;
#1378 = ADVANCED_FACE ( 'NONE', ( #1593 ), #174, .T. ) ;
#1379 =( NAMED_UNIT ( * ) PLANE_ANGLE_UNIT ( ) SI_UNIT ( $, .RADIAN. ) );
#1380 = CYLINDRICAL_SURFACE ( 'NONE', #2470, 4.000000000000000000 ) ;
#1381 = ORIENTED_EDGE ( 'NONE', *, *, #1748, .F. ) ;
#1382 = PRODUCT_DEFINITION_SHAPE ( 'NONE', 'NONE',  #4708 ) ;
#1383 = CARTESIAN_POINT ( 'NONE',  ( 20.67279826512042007, 15.85973458909327860, 20.00001200000000523 ) ) ;
#1384 = VECTOR ( 'NONE', #323, 1000.000000000000000 ) ;
#1385 = DIRECTION ( 'NONE',  ( 0.000000000000000000, 0.000000000000000000, 1.000000000000000000 ) ) ;
#1386 = EDGE_CURVE ( 'NONE', #1279, #1199, #3610, .T. ) ;
#1387 = DIRECTION ( 'NONE',  ( -0.000000000000000000, 1.000000000000000000, -0.000000000000000000 ) ) ;
#1388 = ADVANCED_FACE ( 'NONE', ( #3563 ), #3167, .T. ) ;
#1389 = CARTESIAN_POINT ( 'NONE',  ( 3.179912982098363816, 29.83135056253849626, 11.44055532734088665 ) ) ;
#1390 = AXIS2_PLACEMENT_3D ( 'NONE', #3409, #915, #1300 ) ;
#1391 = CARTESIAN_POINT ( 'NONE',  ( 3.967457472430142573, 31.06577176399945017, 8.474369013652145455 ) ) ;
#1392 = APPLICATION_PROTOCOL_DEFINITION ( 'draft international standard', 'automotive_design', 1998, #4013 ) ;
#1393 = CARTESIAN_POINT ( 'NONE',  ( -6.741346781237202102, -25.16843286583315731, 20.00001200000000168 ) ) ;
#1394 = DIRECTION ( 'NONE',  ( 0.000000000000000000, 0.000000000000000000, 1.000000000000000000 ) ) ;
#1395 = CARTESIAN_POINT ( 'NONE',  ( 0.000000000000000000, 10.00000000000000000, 15.00000000000000178 ) ) ;
#1396 = DIRECTION ( 'NONE',  ( -1.000000000000000000, 0.000000000000000000, 0.000000000000000000 ) ) ;
#1397 = EDGE_LOOP ( 'NONE', ( #999, #2989, #3673, #2512 ) ) ;
#1398 = ORIENTED_EDGE ( 'NONE', *, *, #2495, .F. ) ;
#1399 = EDGE_CURVE ( 'NONE', #310, #3729, #697, .T. ) ;
#1400 = CARTESIAN_POINT ( 'NONE',  ( 3.889087296526035242, 34.17157287525380838, 6.110912703473999841 ) ) ;
#1401 = AXIS2_PLACEMENT_3D ( 'NONE', #655, #1058, #3239 ) ;
#1402 = DIRECTION ( 'NONE',  ( -0.000000000000000000, 1.000000000000000000, -0.000000000000000000 ) ) ;
#1403 = DIRECTION ( 'NONE',  ( 1.000000000000000000, 0.000000000000000000, 0.000000000000000000 ) ) ;
#1404 = EDGE_CURVE ( 'NONE', #1997, #1098, #2874, .T. ) ;
#1405 = ORIENTED_EDGE ( 'NONE', *, *, #3553, .F. ) ;
#1406 = DIRECTION ( 'NONE',  ( 0.000000000000000000, -0.000000000000000000, 1.000000000000000000 ) ) ;
#1407 = PLANE ( 'NONE',  #902 ) ;
#1408 = SHAPE_REPRESENTATION ( 'casing', ( #2928 ), #656 ) ;
#1409 = CARTESIAN_POINT ( 'NONE',  ( -18.19536891688249014, 23.85222316637480233, 8.999999999999992895 ) ) ;
#1410 = LINE ( 'NONE', #1366, #2230 ) ;
#1411 = FACE_OUTER_BOUND ( 'NONE', #3680, .T. ) ;
#1412 = MANIFOLD_SOLID_BREP ( 'Extrude-Thin1', #2143 ) ;
#1413 = AXIS2_PLACEMENT_3D ( 'NONE', #3396, #1582, #757 ) ;
#1414 = FACE_BOUND ( 'NONE', #1684, .T. ) ;
#1415 = ADVANCED_FACE ( 'NONE', ( #1800 ), #2438, .F. ) ;
#1416 = AXIS2_PLACEMENT_3D ( 'NONE', #3968, #2841, #2938 ) ;
#1417 = ADVANCED_FACE ( 'NONE', ( #2830 ), #3975, .F. ) ;
#1418 = CARTESIAN_POINT ( 'NONE',  ( -22.86845070612092456, 19.41857644225268942, 5.819272910265529397 ) ) ;
#1419 = CARTESIAN_POINT ( 'NONE',  ( -26.50000000000000355, -0.5000000000000000000, 19.50000000000000000 ) ) ;
#1420 = DIRECTION ( 'NONE',  ( -0.000000000000000000, 1.000000000000000000, 0.000000000000000000 ) ) ;
#1421 = EDGE_LOOP ( 'NONE', ( #1338, #2203, #4426, #149 ) ) ;
#1422 = ORIENTED_EDGE ( 'NONE', *, *, #1264, .F. ) ;
#1423 = DIRECTION ( 'NONE',  ( 1.224646799147350495E-16, 0.000000000000000000, -1.000000000000000000 ) ) ;
#1424 = PRESENTATION_STYLE_ASSIGNMENT (( #3231 ) ) ;
#1425 = DIRECTION ( 'NONE',  ( 0.000000000000000000, 1.000000000000000000, 0.000000000000000000 ) ) ;
#1426 = ORIENTED_EDGE ( 'NONE', *, *, #1764, .F. ) ;
#1427 = CARTESIAN_POINT ( 'NONE',  ( 23.36965697125207342, 11.52193136556788211, 20.00001200000000523 ) ) ;
#1428 = AXIS2_PLACEMENT_3D ( 'NONE', #3216, #2419, #4656 ) ;
#1429 = CARTESIAN_POINT ( 'NONE',  ( 17.67766952966372429, 17.67766952966365679, 8.999999999999992895 ) ) ;
#1430 = DIRECTION ( 'NONE',  ( 0.000000000000000000, 1.000000000000000000, 0.000000000000000000 ) ) ;
#1431 = DIRECTION ( 'NONE',  ( 1.000000000000000000, 0.000000000000000000, 0.000000000000000000 ) ) ;
#1432 = AXIS2_PLACEMENT_3D ( 'NONE', #1352, #1675, #3152 ) ;
#1433 = LINE ( 'NONE', #2594, #1810 ) ;
#1434 = CARTESIAN_POINT ( 'NONE',  ( 3.672900200782976743, 31.76776247384029972, 7.403954086897937437 ) ) ;
#1435 = EDGE_CURVE ( 'NONE', #3477, #3682, #15, .T. ) ;
#1436 = CARTESIAN_POINT ( 'NONE',  ( 18.29840776695833071, 23.77332420219740072, 7.960232512805602845 ) ) ;
#1437 = CARTESIAN_POINT ( 'NONE',  ( -0.9958591954639161026, 49.00000000000000000, 3.590909090909080170 ) ) ;
#1438 = ADVANCED_FACE ( 'NONE', ( #1777 ), #1735, .T. ) ;
#1439 = CARTESIAN_POINT ( 'NONE',  ( -8.000000000000000000, 10.00000000000000178, 15.00000000000000178 ) ) ;
#1440 = EDGE_CURVE ( 'NONE', #816, #1148, #2412, .T. ) ;
#1441 = EDGE_LOOP ( 'NONE', ( #46, #1980, #4001, #3042 ) ) ;
#1442 = AXIS2_PLACEMENT_3D ( 'NONE', #901, #3806, #1607 ) ;
#1443 = VERTEX_POINT ( 'NONE', #4697 ) ;
#1444 = CARTESIAN_POINT ( 'NONE',  ( -0.5000000000000000000, 6.000000000000000000, 19.50000000000000000 ) ) ;
#1445 =( NAMED_UNIT ( * ) PLANE_ANGLE_UNIT ( ) SI_UNIT ( $, .RADIAN. ) );
#1446 = DIRECTION ( 'NONE',  ( 0.000000000000000000, 0.000000000000000000, 1.000000000000000000 ) ) ;
#1447 = EDGE_LOOP ( 'NONE', ( #2183, #2534, #3731, #160 ) ) ;
#1448 = EDGE_LOOP ( 'NONE', ( #2971, #1183 ) ) ;
#1449 = EDGE_LOOP ( 'NONE', ( #1010, #1696, #3014, #3137, #2336 ) ) ;
#1450 = CARTESIAN_POINT ( 'NONE',  ( -5.499999999999996447, 37.00000000000000000, 8.999999999999992895 ) ) ;
#1451 = CARTESIAN_POINT ( 'NONE',  ( 3.523178763948789705, 33.65307825300501321, 7.105158153061387871 ) ) ;
#1452 = DIRECTION ( 'NONE',  ( 1.000000000000000000, 0.000000000000000000, 0.000000000000000000 ) ) ;
#1453 = EDGE_CURVE ( 'NONE', #1443, #3862, #467, .T. ) ;
#1454 = FACE_OUTER_BOUND ( 'NONE', #2925, .T. ) ;
#1455 = VECTOR ( 'NONE', #3969, 1000.000000000000000 ) ;
#1456 = CARTESIAN_POINT ( 'NONE',  ( 3.871991356174931731, 31.26893492619631942, 10.01005989714294664 ) ) ;
#1457 = SHAPE_DEFINITION_REPRESENTATION ( #4494, #3382 ) ;
#1458 = CARTESIAN_POINT ( 'NONE',  ( 20.83941891177998684, 21.58204166899915322, 5.025993266704736229 ) ) ;
#1459 = CYLINDRICAL_SURFACE ( 'NONE', #4138, 1.000000000000000888 ) ;
#1460 = LINE ( 'NONE', #1, #1273 ) ;
#1461 = ORIENTED_EDGE ( 'NONE', *, *, #407, .T. ) ;
#1462 = ORIENTED_EDGE ( 'NONE', *, *, #84, .F. ) ;
#1463 = CARTESIAN_POINT ( 'NONE',  ( -3.775946040281024541, 31.49506148730309008, 10.32350191120198346 ) ) ;
#1464 = PRODUCT_RELATED_PRODUCT_CATEGORY ( 'part', '', ( #1681 ) ) ;
#1465 = DIRECTION ( 'NONE',  ( -0.000000000000000000, 1.000000000000000000, -0.000000000000000000 ) ) ;
#1466 = VERTEX_POINT ( 'NONE', #4330 ) ;
#1467 = AXIS2_PLACEMENT_3D ( 'NONE', #2402, #3508, #4585 ) ;
#1468 = VERTEX_POINT ( 'NONE', #1444 ) ;
#1469 = ORIENTED_EDGE ( 'NONE', *, *, #3532, .F. ) ;
#1470 = DIRECTION ( 'NONE',  ( 0.000000000000000000, 1.000000000000000000, 0.000000000000000000 ) ) ;
#1471 = CARTESIAN_POINT ( 'NONE',  ( -23.23784379901361419, 18.97463723504665367, 11.64206388705991557 ) ) ;
#1472 = TOROIDAL_SURFACE ( 'NONE', #955, 3.000000000000002665, 1.749999999999999778 ) ;
#1473 =( NAMED_UNIT ( * ) PLANE_ANGLE_UNIT ( ) SI_UNIT ( $, .RADIAN. ) );
#1474 = DIRECTION ( 'NONE',  ( -0.000000000000000000, -1.000000000000000000, -0.000000000000000000 ) ) ;
#1475 = ORIENTED_EDGE ( 'NONE', *, *, #86, .T. ) ;
#1476 = CYLINDRICAL_SURFACE ( 'NONE', #225, 0.5000000000000001110 ) ;
#1477 = COLOUR_RGB ( '',0.8941176470588234615, 0.8941176470588234615, 0.8941176470588234615 ) ;
#1478 = CARTESIAN_POINT ( 'NONE',  ( -0.9958591954639913757, 43.00000000000000000, 14.40909090909089230 ) ) ;
#1479 = CONTEXT_DEPENDENT_SHAPE_REPRESENTATION ( #1551, #1988 ) ;
#1480 = CIRCLE ( 'NONE', #4233, 0.5000000000000000000 ) ;
#1481 =( REPRESENTATION_RELATIONSHIP ('NONE','NONE', #2397, #3050 ) REPRESENTATION_RELATIONSHIP_WITH_TRANSFORMATION ( #1815 )SHAPE_REPRESENTATION_RELATIONSHIP( ) );
#1482 = CARTESIAN_POINT ( 'NONE',  ( 18.51843501006192483, 23.60249532755118551, 7.226626843687536272 ) ) ;
#1483 = DIRECTION ( 'NONE',  ( 0.000000000000000000, 0.000000000000000000, 1.000000000000000000 ) ) ;
#1484 = CARTESIAN_POINT ( 'NONE',  ( -8.999999999999973355, 32.99999999999999289, 1.749999999999999778 ) ) ;
#1485 = VERTEX_POINT ( 'NONE', #626 ) ;
#1486 = EDGE_LOOP ( 'NONE', ( #4239, #3021, #2201, #1426 ) ) ;
#1487 = CARTESIAN_POINT ( 'NONE',  ( -3.809567799457745263, 31.41347316107661314, 10.22463024623739081 ) ) ;
#1488 = SURFACE_STYLE_FILL_AREA ( #739 ) ;
#1489 = CYLINDRICAL_SURFACE ( 'NONE', #921, 5.000000000000001776 ) ;
#1490 = VERTEX_POINT ( 'NONE', #3517 ) ;
#1491 = EDGE_LOOP ( 'NONE', ( #4387, #919, #947, #2244 ) ) ;
#1492 = EDGE_LOOP ( 'NONE', ( #3105, #3631 ) ) ;
#1493 = CARTESIAN_POINT ( 'NONE',  ( 3.120626071653123113, 43.00000000000000000, 13.52898365209223996 ) ) ;
#1494 = CARTESIAN_POINT ( 'NONE',  ( -20.47065640071377501, 21.93211642885832191, 12.87299606428841159 ) ) ;
#1495 = ADVANCED_FACE ( 'NONE', ( #262 ), #1093, .T. ) ;
#1496 = CARTESIAN_POINT ( 'NONE',  ( -26.00000000000000355, 0.000000000000000000, 19.59999999999999787 ) ) ;
#1497 = FACE_OUTER_BOUND ( 'NONE', #2181, .T. ) ;
#1498 = EDGE_LOOP ( 'NONE', ( #4018, #1047, #3591, #736 ) ) ;
#1499 = LINE ( 'NONE', #37, #3410 ) ;
#1500 = AXIS2_PLACEMENT_3D ( 'NONE', #106, #1546, #2298 ) ;
#1501 = CARTESIAN_POINT ( 'NONE',  ( 26.49999999999999645, 0.5000000000000000000, 19.50000000000000000 ) ) ;
#1502 = MECHANICAL_DESIGN_GEOMETRIC_PRESENTATION_REPRESENTATION (  '', ( #2330 ), #3637 ) ;
#1503 = CARTESIAN_POINT ( 'NONE',  ( 0.000000000000000000, 0.000000000000000000, 15.00000000000000178 ) ) ;
#1504 = DIRECTION ( 'NONE',  ( 1.000000000000000000, 0.000000000000000000, 0.000000000000000000 ) ) ;
#1505 = AXIS2_PLACEMENT_3D ( 'NONE', #1056, #3963, #610 ) ;
#1506 = DIRECTION ( 'NONE',  ( -0.000000000000000000, -0.000000000000000000, -1.000000000000000000 ) ) ;
#1507 = VERTEX_POINT ( 'NONE', #2528 ) ;
#1508 = ORIENTED_EDGE ( 'NONE', *, *, #3086, .T. ) ;
#1509 = VECTOR ( 'NONE', #4292, 1000.000000000000000 ) ;
#1510 = CYLINDRICAL_SURFACE ( 'NONE', #2136, 5.500000000000000000 ) ;
#1511 =( NAMED_UNIT ( * ) SI_UNIT ( $, .STERADIAN. ) SOLID_ANGLE_UNIT ( ) );
#1512 = FACE_OUTER_BOUND ( 'NONE', #2383, .T. ) ;
#1513 = VERTEX_POINT ( 'NONE', #2580 ) ;
#1514 = EDGE_LOOP ( 'NONE', ( #2227, #2318, #2635, #3413 ) ) ;
#1515 = ORIENTED_EDGE ( 'NONE', *, *, #3618, .F. ) ;
#1516 = DIRECTION ( 'NONE',  ( 0.000000000000000000, 0.000000000000000000, 1.000000000000000000 ) ) ;
#1517 = EDGE_CURVE ( 'NONE', #2090, #2680, #1682, .T. ) ;
#1518 = TOROIDAL_SURFACE ( 'NONE', #90, 4.000000000000001776, 1.000000000000000000 ) ;
#1519 = CARTESIAN_POINT ( 'NONE',  ( -18.29899638405149886, 23.77287215665554143, 10.04298872102888751 ) ) ;
#1520 = EDGE_CURVE ( 'NONE', #2903, #3494, #4336, .T. ) ;
#1521 = CARTESIAN_POINT ( 'NONE',  ( 26.00000000000000711, 3.184081677783118980E-15, 19.50000000000000000 ) ) ;
#1522 = LINE ( 'NONE', #1172, #2936 ) ;
#1523 = ORIENTED_EDGE ( 'NONE', *, *, #227, .F. ) ;
#1524 = EDGE_CURVE ( 'NONE', #4308, #3204, #1923, .T. ) ;
#1525 = FACE_OUTER_BOUND ( 'NONE', #1105, .T. ) ;
#1526 = ADVANCED_FACE ( 'NONE', ( #4069, #1823 ), #805, .F. ) ;
#1527 = CIRCLE ( 'NONE', #2744, 4.000000000000000000 ) ;
#1528 = CARTESIAN_POINT ( 'NONE',  ( -27.10000000000000497, -0.5999999999999998668, 19.59999999999999787 ) ) ;
#1529 = CIRCLE ( 'NONE', #2070, 26.00000000000000711 ) ;
#1530 = B_SPLINE_CURVE_WITH_KNOTS ( 'NONE', 3,
 ( #321, #3686, #4386, #33, #2232, #3309, #1128, #2129, #1832, #1152, #2474, #2931, #4408, #2590, #1393, #2426, #2566, #2082, #2451, #4031, #3551, #3333, #1016, #771, #2207, #1042, #3916, #1724, #1857, #4254, #3665, #300, #1747, #3198 ),
 .UNSPECIFIED., .F., .F.,
 ( 4, 2, 2, 2, 2, 2, 2, 2, 2, 2, 2, 2, 2, 2, 2, 2, 4 ),
 ( 0.5000000000000000000, 0.5312500000000000000, 0.5625000000000000000, 0.5937500000000000000, 0.6250000000000000000, 0.6562500000000000000, 0.6875000000000000000, 0.7187500000000000000, 0.7500000000000000000, 0.7812500000000000000, 0.8125000000000000000, 0.8437500000000000000, 0.8750000000000000000, 0.9062500000000000000, 0.9375000000000000000, 0.9687500000000000000, 1.000000000000000000 ),
 .UNSPECIFIED. ) ;
#1531 = DIRECTION ( 'NONE',  ( -0.000000000000000000, -1.000000000000000000, -0.000000000000000000 ) ) ;
#1532 = FACE_OUTER_BOUND ( 'NONE', #76, .T. ) ;
#1533 = DIRECTION ( 'NONE',  ( 0.000000000000000000, -1.000000000000000000, -0.000000000000000000 ) ) ;
#1534 = AXIS2_PLACEMENT_3D ( 'NONE', #4579, #4267, #1007 ) ;
#1535 = ORIENTED_EDGE ( 'NONE', *, *, #2027, .T. ) ;
#1536 = ORIENTED_EDGE ( 'NONE', *, *, #3804, .T. ) ;
#1537 = DIRECTION ( 'NONE',  ( 1.000000000000000000, 0.000000000000000000, 0.000000000000000000 ) ) ;
#1538 = DIRECTION ( 'NONE',  ( 0.000000000000000000, 1.000000000000000000, 0.000000000000000000 ) ) ;
#1539 = FILL_AREA_STYLE ('',( #3348 ) ) ;
#1540 = DIRECTION ( 'NONE',  ( 0.000000000000000000, 1.000000000000000000, 0.000000000000000000 ) ) ;
#1541 = EDGE_LOOP ( 'NONE', ( #3473, #2533, #2637, #3666 ) ) ;
#1542 = ORIENTED_EDGE ( 'NONE', *, *, #1131, .T. ) ;
#1543 = VERTEX_POINT ( 'NONE', #2967 ) ;
#1544 = ORIENTED_EDGE ( 'NONE', *, *, #2306, .T. ) ;
#1545 = UNCERTAINTY_MEASURE_WITH_UNIT (LENGTH_MEASURE( 1.000000000000000082E-05 ), #651, 'distance_accuracy_value', 'NONE');
#1546 = DIRECTION ( 'NONE',  ( -0.000000000000000000, -1.000000000000000000, -0.000000000000000000 ) ) ;
#1547 = DIRECTION ( 'NONE',  ( 0.000000000000000000, 0.000000000000000000, 1.000000000000000000 ) ) ;
#1548 = EDGE_CURVE ( 'NONE', #1588, #3303, #2283, .T. ) ;
#1549 = DIRECTION ( 'NONE',  ( 0.000000000000000000, 1.000000000000000000, 0.000000000000000000 ) ) ;
#1550 = VERTEX_POINT ( 'NONE', #1847 ) ;
#1551 =( REPRESENTATION_RELATIONSHIP ('NONE','NONE', #2397, #404 ) REPRESENTATION_RELATIONSHIP_WITH_TRANSFORMATION ( #3290 )SHAPE_REPRESENTATION_RELATIONSHIP( ) );
#1552 = LINE ( 'NONE', #461, #472 ) ;
#1553 = DIRECTION ( 'NONE',  ( 0.000000000000000000, 1.000000000000000000, 0.000000000000000000 ) ) ;
#1554 = AXIS2_PLACEMENT_3D ( 'NONE', #3843, #2742, #3798 ) ;
#1555 = PRODUCT_DEFINITION ( 'UNKNOWN', '', #207, #3519 ) ;
#1556 = EDGE_CURVE ( 'NONE', #1279, #1651, #3779, .T. ) ;
#1557 = LINE ( 'NONE', #515, #1256 ) ;
#1558 = CARTESIAN_POINT ( 'NONE',  ( -3.471741185006985919, 33.26424185130363043, 10.98693824102217498 ) ) ;
#1559 = COLOUR_RGB ( '',0.8941176470588234615, 0.8941176470588234615, 0.8941176470588234615 ) ;
#1560 = VERTEX_POINT ( 'NONE', #419 ) ;
#1561 = EDGE_CURVE ( 'NONE', #3402, #52, #243, .T. ) ;
#1562 = CARTESIAN_POINT ( 'NONE',  ( 0.000000000000000000, 0.000000000000000000, 15.00000000000000178 ) ) ;
#1563 = DIRECTION ( 'NONE',  ( 1.000000000000000000, 0.000000000000000000, 0.000000000000000000 ) ) ;
#1564 = PRODUCT_DEFINITION_SHAPE ( 'NONE', 'NONE',  #3507 ) ;
#1565 = CARTESIAN_POINT ( 'NONE',  ( 0.000000000000000000, 10.00000000000000000, -2.999999999999999112 ) ) ;
#1566 = CIRCLE ( 'NONE', #3162, 1.750000000000001554 ) ;
#1567 = DIRECTION ( 'NONE',  ( 0.000000000000000000, 0.000000000000000000, 1.000000000000000000 ) ) ;
#1568 = ORIENTED_EDGE ( 'NONE', *, *, #2355, .F. ) ;
#1569 = EDGE_LOOP ( 'NONE', ( #194, #965, #2792, #1274 ) ) ;
#1570 = ORIENTED_EDGE ( 'NONE', *, *, #516, .T. ) ;
#1571 = ORIENTED_EDGE ( 'NONE', *, *, #2927, .T. ) ;
#1572 = DIRECTION ( 'NONE',  ( 0.000000000000000000, 0.000000000000000000, 1.000000000000000000 ) ) ;
#1573 = CARTESIAN_POINT ( 'NONE',  ( -22.58509718322855164, 19.74742367678131316, 12.47015313278852666 ) ) ;
#1574 = UNCERTAINTY_MEASURE_WITH_UNIT (LENGTH_MEASURE( 1.000000000000000082E-05 ), #1723, 'distance_accuracy_value', 'NONE');
#1575 = FACE_OUTER_BOUND ( 'NONE', #2932, .T. ) ;
#1576 = EDGE_LOOP ( 'NONE', ( #4394, #4173 ) ) ;
#1577 = CARTESIAN_POINT ( 'NONE',  ( 24.00000000000000355, 0.000000000000000000, 17.00000000000000000 ) ) ;
#1578 = DIRECTION ( 'NONE',  ( -0.000000000000000000, -1.000000000000000000, -0.000000000000000000 ) ) ;
#1579 = AXIS2_PLACEMENT_3D ( 'NONE', #1616, #2659, #4176 ) ;
#1580 = ADVANCED_FACE ( 'NONE', ( #3654 ), #1510, .T. ) ;
#1581 = DIRECTION ( 'NONE',  ( 0.000000000000000000, 0.000000000000000000, 1.000000000000000000 ) ) ;
#1582 = DIRECTION ( 'NONE',  ( -0.000000000000000000, -1.000000000000000000, -0.000000000000000000 ) ) ;
#1583 = ADVANCED_FACE ( 'NONE', ( #2674 ), #4204, .T. ) ;
#1584 = CARTESIAN_POINT ( 'NONE',  ( -18.19536891688249014, 23.85222316637480233, 8.999999999999992895 ) ) ;
#1585 = CARTESIAN_POINT ( 'NONE',  ( 3.993355759804221083, 34.98680951811717676, 8.734987511292612083 ) ) ;
#1586 = EDGE_CURVE ( 'NONE', #2135, #289, #1654, .T. ) ;
#1587 = LINE ( 'NONE', #3018, #4415 ) ;
#1588 = VERTEX_POINT ( 'NONE', #3015 ) ;
#1589 = ORIENTED_EDGE ( 'NONE', *, *, #1874, .F. ) ;
#1590 = ORIENTED_EDGE ( 'NONE', *, *, #2926, .F. ) ;
#1591 = ORIENTED_EDGE ( 'NONE', *, *, #142, .T. ) ;
#1592 = DIRECTION ( 'NONE',  ( 0.000000000000000000, -1.000000000000000000, 0.000000000000000000 ) ) ;
#1593 = FACE_OUTER_BOUND ( 'NONE', #417, .T. ) ;
#1594 = SURFACE_SIDE_STYLE ('',( #154 ) ) ;
#1595 = FILL_AREA_STYLE ('',( #3791 ) ) ;
#1596 = CYLINDRICAL_SURFACE ( 'NONE', #4640, 5.500000000000000000 ) ;
#1597 = AXIS2_PLACEMENT_3D ( 'NONE', #97, #119, #396 ) ;
#1598 = DIRECTION ( 'NONE',  ( 0.000000000000000000, 0.000000000000000000, 1.000000000000000000 ) ) ;
#1599 = DIRECTION ( 'NONE',  ( 0.000000000000000000, 0.000000000000000000, -1.000000000000000000 ) ) ;
#1600 = EDGE_CURVE ( 'NONE', #3514, #4523, #2273, .T. ) ;
#1601 = DIRECTION ( 'NONE',  ( 0.000000000000000000, 0.000000000000000000, -1.000000000000000000 ) ) ;
#1602 = VERTEX_POINT ( 'NONE', #3440 ) ;
#1603 = ADVANCED_FACE ( 'NONE', ( #3825 ), #493, .T. ) ;
#1604 = CARTESIAN_POINT ( 'NONE',  ( -3.794751686895379894, 29.75919970560060079, 7.708599238039753665 ) ) ;
#1605 = CARTESIAN_POINT ( 'NONE',  ( 0.000000000000000000, 10.00000000000000000, 17.00000000000000000 ) ) ;
#1606 = VECTOR ( 'NONE', #2974, 1000.000000000000000 ) ;
#1607 = DIRECTION ( 'NONE',  ( 1.000000000000000000, 0.000000000000000000, 0.000000000000000000 ) ) ;
#1608 = CARTESIAN_POINT ( 'NONE',  ( 3.575798854573977614, 33.89464632526108545, 10.79358726550606029 ) ) ;
#1609 = AXIS2_PLACEMENT_3D ( 'NONE', #702, #744, #2587 ) ;
#1610 = DIRECTION ( 'NONE',  ( 1.000000000000000000, 0.000000000000000000, 0.000000000000000000 ) ) ;
#1611 = CARTESIAN_POINT ( 'NONE',  ( 3.889087296526035242, 34.17157287525380838, 5.110912703473999841 ) ) ;
#1612 = ORIENTED_EDGE ( 'NONE', *, *, #3207, .T. ) ;
#1613 = ORIENTED_EDGE ( 'NONE', *, *, #3132, .F. ) ;
#1614 = VERTEX_POINT ( 'NONE', #3113 ) ;
#1615 = EDGE_LOOP ( 'NONE', ( #3368, #3959, #2654, #1090 ) ) ;
#1616 = CARTESIAN_POINT ( 'NONE',  ( -1.734723475976807094E-15, 45.00000000000000000, 0.000000000000000000 ) ) ;
#1617 = ADVANCED_FACE ( 'NONE', ( #3851 ), #164, .T. ) ;
#1618 = CARTESIAN_POINT ( 'NONE',  ( 0.000000000000000000, 0.000000000000000000, 19.59999999999999787 ) ) ;
#1619 =( LENGTH_UNIT ( ) NAMED_UNIT ( * ) SI_UNIT ( .MILLI., .METRE. ) );
#1620 = EDGE_CURVE ( 'NONE', #2966, #2780, #3749, .T. ) ;
#1621 = LINE ( 'NONE', #3073, #3384 ) ;
#1622 = LINE ( 'NONE', #2664, #247 ) ;
#1623 = LINE ( 'NONE', #4462, #2436 ) ;
#1624 = CYLINDRICAL_SURFACE ( 'NONE', #451, 5.500000000000000000 ) ;
#1625 = CARTESIAN_POINT ( 'NONE',  ( 3.959305671612554781E-15, 25.00000000000000000, 12.99999999999999289 ) ) ;
#1626 = ORIENTED_EDGE ( 'NONE', *, *, #1131, .F. ) ;
#1627 = VECTOR ( 'NONE', #1278, 1000.000000000000000 ) ;
#1628 = LINE ( 'NONE', #4189, #3221 ) ;
#1629 = CARTESIAN_POINT ( 'NONE',  ( -0.5000000000000000000, 0.000000000000000000, 20.00000000000000000 ) ) ;
#1630 = DIRECTION ( 'NONE',  ( 0.000000000000000000, 1.000000000000000000, -0.000000000000000000 ) ) ;
#1631 = DIRECTION ( 'NONE',  ( 0.000000000000000000, 0.000000000000000000, 1.000000000000000000 ) ) ;
#1632 = SHAPE_REPRESENTATION_RELATIONSHIP ( 'NONE' , 'NONE' ,  #4641, #4382 ) ;
#1633 = CARTESIAN_POINT ( 'NONE',  ( -23.36965697125209473, 11.52193136556784481, 20.00001200000000168 ) ) ;
#1634 = ORIENTED_EDGE ( 'NONE', *, *, #1250, .F. ) ;
#1635 = ORIENTED_EDGE ( 'NONE', *, *, #3271, .F. ) ;
#1636 = ORIENTED_EDGE ( 'NONE', *, *, #1764, .T. ) ;
#1637 = ORIENTED_EDGE ( 'NONE', *, *, #1561, .F. ) ;
#1638 = CARTESIAN_POINT ( 'NONE',  ( -0.7500000000000001110, 0.000000000000000000, 18.19999999999999929 ) ) ;
#1639 = MECHANICAL_DESIGN_GEOMETRIC_PRESENTATION_REPRESENTATION (  '', ( #4159 ), #4692 ) ;
#1640 = LINE ( 'NONE', #4503, #161 ) ;
#1641 = PRESENTATION_STYLE_ASSIGNMENT (( #1247 ) ) ;
#1642 =( LENGTH_UNIT ( ) NAMED_UNIT ( * ) SI_UNIT ( .MILLI., .METRE. ) );
#1643 = VERTEX_POINT ( 'NONE', #3398 ) ;
#1644 = PRESENTATION_LAYER_ASSIGNMENT (  '', '', ( #1718 ) ) ;
#1645 = AXIS2_PLACEMENT_3D ( 'NONE', #4289, #353, #740 ) ;
#1646 = DIRECTION ( 'NONE',  ( 1.000000000000000000, 0.000000000000000000, 0.000000000000000000 ) ) ;
#1647 = EDGE_CURVE ( 'NONE', #1602, #4361, #4265, .T. ) ;
#1648 = DIRECTION ( 'NONE',  ( 0.000000000000000000, 0.000000000000000000, 1.000000000000000000 ) ) ;
#1649 = FACE_OUTER_BOUND ( 'NONE', #3543, .T. ) ;
#1650 = EDGE_CURVE ( 'NONE', #2657, #4199, #1527, .T. ) ;
#1651 = VERTEX_POINT ( 'NONE', #210 ) ;
#1652 = CARTESIAN_POINT ( 'NONE',  ( 18.61605759292315199, 23.52581488222641326, 11.00403192580902711 ) ) ;
#1653 = DIRECTION ( 'NONE',  ( 1.000000000000000000, -0.000000000000000000, -0.000000000000000000 ) ) ;
#1654 = LINE ( 'NONE', #4538, #2056 ) ;
#1655 = AXIS2_PLACEMENT_3D ( 'NONE', #4621, #2387, #2828 ) ;
#1656 = DIRECTION ( 'NONE',  ( 0.000000000000000000, 0.000000000000000000, 1.000000000000000000 ) ) ;
#1657 = DIRECTION ( 'NONE',  ( 0.000000000000000000, 0.000000000000000000, 1.000000000000000000 ) ) ;
#1658 = ORIENTED_EDGE ( 'NONE', *, *, #4037, .F. ) ;
#1659 = EDGE_LOOP ( 'NONE', ( #4477, #4218 ) ) ;
#1660 = EDGE_LOOP ( 'NONE', ( #3022, #4009, #2737, #3858 ) ) ;
#1661 = EDGE_CURVE ( 'NONE', #907, #2288, #705, .T. ) ;
#1662 = VECTOR ( 'NONE', #3899, 1000.000000000000000 ) ;
#1663 = DIRECTION ( 'NONE',  ( -1.000000000000000000, -0.000000000000000000, -0.000000000000000000 ) ) ;
#1664 = CARTESIAN_POINT ( 'NONE',  ( -8.999999999999998224, 36.00000000000000711, 0.000000000000000000 ) ) ;
#1665 = LINE ( 'NONE', #2004, #1342 ) ;
#1666 = AXIS2_PLACEMENT_3D ( 'NONE', #211, #186, #1656 ) ;
#1667 = ORIENTED_EDGE ( 'NONE', *, *, #777, .F. ) ;
#1668 = DIRECTION ( 'NONE',  ( -0.000000000000000000, -1.000000000000000000, -0.000000000000000000 ) ) ;
#1669 = CARTESIAN_POINT ( 'NONE',  ( 0.000000000000000000, 0.000000000000000000, 17.69999999999999929 ) ) ;
#1670 = ADVANCED_FACE ( 'NONE', ( #4567 ), #951, .F. ) ;
#1671 = CARTESIAN_POINT ( 'NONE',  ( -0.7500000000000000000, -2.999999999999999556, 17.69999999999999929 ) ) ;
#1672 = DIRECTION ( 'NONE',  ( 0.000000000000000000, 0.000000000000000000, 1.000000000000000000 ) ) ;
#1673 = ORIENTED_EDGE ( 'NONE', *, *, #3531, .T. ) ;
#1674 = PRESENTATION_LAYER_ASSIGNMENT (  '', '', ( #2667 ) ) ;
#1675 = DIRECTION ( 'NONE',  ( -0.000000000000000000, -1.000000000000000000, -0.000000000000000000 ) ) ;
#1676 = PRODUCT_RELATED_PRODUCT_CATEGORY ( 'part', '', ( #2064 ) ) ;
#1677 = DIRECTION ( 'NONE',  ( -0.000000000000000000, 0.000000000000000000, 1.000000000000000000 ) ) ;
#1678 = DIRECTION ( 'NONE',  ( 0.000000000000000000, 1.000000000000000000, 0.000000000000000000 ) ) ;
#1679 = CYLINDRICAL_SURFACE ( 'NONE', #937, 1.000000000000000000 ) ;
#1680 = CYLINDRICAL_SURFACE ( 'NONE', #3112, 1.500000000000000222 ) ;
#1681 = PRODUCT ( 'stop button', 'stop button', '', ( #320 ) ) ;
#1682 = CIRCLE ( 'NONE', #2430, 24.00000000000000355 ) ;
#1683 = CARTESIAN_POINT ( 'NONE',  ( -11.52193136556785369, 23.36965697125208052, 20.00001200000000168 ) ) ;
#1684 = EDGE_LOOP ( 'NONE', ( #501, #1523 ) ) ;
#1685 = ORIENTED_EDGE ( 'NONE', *, *, #3593, .T. ) ;
#1686 = ORIENTED_EDGE ( 'NONE', *, *, #3741, .T. ) ;
#1687 = DIRECTION ( 'NONE',  ( 0.000000000000000000, 0.000000000000000000, 1.000000000000000000 ) ) ;
#1688 = AXIS2_PLACEMENT_3D ( 'NONE', #4667, #1726, #4615 ) ;
#1689 = CARTESIAN_POINT ( 'NONE',  ( 3.469446951953614189E-15, 33.00000000000000000, 4.999999999999992006 ) ) ;
#1690 = FILL_AREA_STYLE_COLOUR ( '', #1111 ) ;
#1691 = DIRECTION ( 'NONE',  ( 1.000000000000000000, 0.000000000000000000, -0.000000000000000000 ) ) ;
#1692 = DIRECTION ( 'NONE',  ( -0.000000000000000000, -0.000000000000000000, 1.000000000000000000 ) ) ;
#1693 = FACE_OUTER_BOUND ( 'NONE', #172, .T. ) ;
#1694 = CARTESIAN_POINT ( 'NONE',  ( 3.469446951953614189E-15, 41.00000000000000000, 8.999999999999992895 ) ) ;
#1695 = FACE_OUTER_BOUND ( 'NONE', #2068, .T. ) ;
#1696 = ORIENTED_EDGE ( 'NONE', *, *, #4086, .F. ) ;
#1697 = CARTESIAN_POINT ( 'NONE',  ( 0.7500000000000001110, 0.000000000000000000, 17.69999999999999929 ) ) ;
#1698 = CARTESIAN_POINT ( 'NONE',  ( 22.10492369241847044, 20.28376480839707341, 12.79609622574099070 ) ) ;
#1699 = CARTESIAN_POINT ( 'NONE',  ( 0.7500000000000001110, 1.299038105676658450, 18.19999999999999929 ) ) ;
#1700 = EDGE_CURVE ( 'NONE', #3253, #906, #4464, .T. ) ;
#1701 = AXIS2_PLACEMENT_3D ( 'NONE', #385, #2284, #1176 ) ;
#1702 = ADVANCED_FACE ( 'NONE', ( #689 ), #1679, .T. ) ;
#1703 = EDGE_CURVE ( 'NONE', #1315, #2022, #100, .T. ) ;
#1704 = CARTESIAN_POINT ( 'NONE',  ( -27.99999999999999645, 0.000000000000000000, 20.00000000000000000 ) ) ;
#1705 = DIRECTION ( 'NONE',  ( 0.000000000000000000, 0.000000000000000000, 1.000000000000000000 ) ) ;
#1706 = DIRECTION ( 'NONE',  ( -0.000000000000000000, -0.000000000000000000, -1.000000000000000000 ) ) ;
#1707 = AXIS2_PLACEMENT_3D ( 'NONE', #791, #1127, #1452 ) ;
#1708 = EDGE_LOOP ( 'NONE', ( #3770, #2507, #1313, #2365 ) ) ;
#1709 = EDGE_LOOP ( 'NONE', ( #1911, #4314 ) ) ;
#1710 = CARTESIAN_POINT ( 'NONE',  ( 0.000000000000000000, 10.00000000000000000, 13.00000000000000178 ) ) ;
#1711 = DIRECTION ( 'NONE',  ( 1.000000000000000000, -0.000000000000000000, -0.000000000000000000 ) ) ;
#1712 = DIRECTION ( 'NONE',  ( 0.000000000000000000, 0.000000000000000000, 1.000000000000000000 ) ) ;
#1713 = PRODUCT_DEFINITION_CONTEXT ( 'detailed design', #3498, 'design' ) ;
#1714 = CARTESIAN_POINT ( 'NONE',  ( 25.16843286583313599, 6.741346781237259833, 20.00001200000000523 ) ) ;
#1715 = FACE_OUTER_BOUND ( 'NONE', #1486, .T. ) ;
#1716 = CARTESIAN_POINT ( 'NONE',  ( -27.10000000000000497, -0.5999999999999998668, 19.59999999999999787 ) ) ;
#1717 = CARTESIAN_POINT ( 'NONE',  ( 8.999999999999966249, 31.24999999999999645, 0.000000000000000000 ) ) ;
#1718 = STYLED_ITEM ( 'NONE', ( #2222 ), #3296 ) ;
#1719 = ORIENTED_EDGE ( 'NONE', *, *, #4105, .T. ) ;
#1720 = CIRCLE ( 'NONE', #1645, 30.00000000000000355 ) ;
#1721 = DIRECTION ( 'NONE',  ( 0.000000000000000000, 0.000000000000000000, 1.000000000000000000 ) ) ;
#1722 = CARTESIAN_POINT ( 'NONE',  ( 23.77287215665559827, 18.29899638405141715, 10.04298872102887863 ) ) ;
#1723 =( LENGTH_UNIT ( ) NAMED_UNIT ( * ) SI_UNIT ( .MILLI., .METRE. ) );
#1724 = CARTESIAN_POINT ( 'NONE',  ( 22.56362157461194329, -13.02991752792603819, 20.00001200000000523 ) ) ;
#1725 = EDGE_CURVE ( 'NONE', #803, #177, #553, .T. ) ;
#1726 = DIRECTION ( 'NONE',  ( 1.621111868633889227E-15, 1.000000000000000000, 0.000000000000000000 ) ) ;
#1727 = DIRECTION ( 'NONE',  ( -1.428364815747576977E-15, -1.000000000000000000, 0.000000000000000000 ) ) ;
#1728 = CARTESIAN_POINT ( 'NONE',  ( -3.601840573626707176, 34.01414095348192035, 7.256529352857233661 ) ) ;
#1729 = ORIENTED_EDGE ( 'NONE', *, *, #4212, .F. ) ;
#1730 = ORIENTED_EDGE ( 'NONE', *, *, #2329, .T. ) ;
#1731 = EDGE_CURVE ( 'NONE', #310, #2780, #173, .T. ) ;
#1732 = AXIS2_PLACEMENT_3D ( 'NONE', #1853, #1470, #3617 ) ;
#1733 = CARTESIAN_POINT ( 'NONE',  ( 26.49999999999999645, -0.5000000000000000000, 19.50000000000000000 ) ) ;
#1734 = B_SPLINE_CURVE_WITH_KNOTS ( 'NONE', 3,
 ( #3684, #107, #31, #431, #2186, #1908, #2999, #3285, #1471, #840, #2278, #1573, #3329, #4381, #4429, #2563, #814, #4125, #3307, #1494, #3734, #4029, #1151, #2256, #1854, #2205, #769, #480, #2930, #3663, #1519, #4077, #81, #1932 ),
 .UNSPECIFIED., .F., .F.,
 ( 4, 2, 2, 2, 2, 2, 2, 2, 2, 2, 2, 2, 2, 2, 2, 2, 4 ),
 ( 0.01251975318912558130, 0.01330204881184919238, 0.01408434443457280347, 0.01486664005729641282, 0.01564893568002002217, 0.01643123130274363325, 0.01721352692546724433, 0.01799582254819085542, 0.01877811817091446650, 0.01956041379363807758, 0.02034270941636168867, 0.02112500503908529975, 0.02190730066180891084, 0.02268959628453252192, 0.02347189190725612953, 0.02425418752997974062, 0.02503648315270335170 ),
 .UNSPECIFIED. ) ;
#1735 = CYLINDRICAL_SURFACE ( 'NONE', #4489, 5.500000000000000000 ) ;
#1736 = SURFACE_STYLE_FILL_AREA ( #672 ) ;
#1737 = VERTEX_POINT ( 'NONE', #3177 ) ;
#1738 = DIRECTION ( 'NONE',  ( 1.000000000000000000, 0.000000000000000000, -0.000000000000000000 ) ) ;
#1739 = CARTESIAN_POINT ( 'NONE',  ( 0.000000000000000000, 0.000000000000000000, 17.69999999999999929 ) ) ;
#1740 = AXIS2_PLACEMENT_3D ( 'NONE', #3238, #1430, #2441 ) ;
#1741 = CARTESIAN_POINT ( 'NONE',  ( -25.99519186311192342, 0.5000000000000000000, 19.50000000000000000 ) ) ;
#1742 = CARTESIAN_POINT ( 'NONE',  ( 2.642082718872652780, 29.88400461830718058, 12.01452573847769045 ) ) ;
#1743 = PRESENTATION_STYLE_ASSIGNMENT (( #637 ) ) ;
#1744 = EDGE_CURVE ( 'NONE', #3472, #1957, #2503, .T. ) ;
#1745 = CARTESIAN_POINT ( 'NONE',  ( 23.23549755865092337, 18.97751144565066994, 11.64625228532890411 ) ) ;
#1746 = ITEM_DEFINED_TRANSFORMATION ( 'NONE', 'NONE', #3088,  #2928 ) ;
#1747 = CARTESIAN_POINT ( 'NONE',  ( 26.00000000000000711, -1.701696020694468015, 20.00001200000000168 ) ) ;
#1748 = EDGE_CURVE ( 'NONE', #1466, #2542, #2354, .T. ) ;
#1749 = AXIS2_PLACEMENT_3D ( 'NONE', #1664, #1296, #3121 ) ;
#1750 = ADVANCED_FACE ( 'NONE', ( #3579, #2845 ), #4304, .T. ) ;
#1751 = CARTESIAN_POINT ( 'NONE',  ( -23.77332420219745757, 18.29840776695824900, 7.960232512805597516 ) ) ;
#1752 = LINE ( 'NONE', #713, #3072 ) ;
#1753 = DIRECTION ( 'NONE',  ( 1.000000000000000000, 0.000000000000000000, -0.000000000000000000 ) ) ;
#1754 = ORIENTED_EDGE ( 'NONE', *, *, #3245, .T. ) ;
#1755 = ORIENTED_EDGE ( 'NONE', *, *, #2918, .T. ) ;
#1756 = CARTESIAN_POINT ( 'NONE',  ( 26.49999999999999645, 0.5000000000000000000, 19.50000000000000000 ) ) ;
#1757 = CARTESIAN_POINT ( 'NONE',  ( 5.500000000000003553, 37.00000000000000000, 8.999999999999992895 ) ) ;
#1758 = FACE_OUTER_BOUND ( 'NONE', #3994, .T. ) ;
#1759 = VERTEX_POINT ( 'NONE', #1332 ) ;
#1760 = LINE ( 'NONE', #1029, #456 ) ;
#1761 = TOROIDAL_SURFACE ( 'NONE', #4422, 4.000000000000001776, 1.000000000000000000 ) ;
#1762 = EDGE_CURVE ( 'NONE', #2297, #2553, #996, .T. ) ;
#1763 = FACE_OUTER_BOUND ( 'NONE', #3403, .T. ) ;
#1764 = EDGE_CURVE ( 'NONE', #2296, #1239, #2774, .T. ) ;
#1765 = PLANE ( 'NONE',  #1428 ) ;
#1766 = CARTESIAN_POINT ( 'NONE',  ( -10.25000000000000178, 44.99999999999999289, 2.143131898507868051E-16 ) ) ;
#1767 = CIRCLE ( 'NONE', #3822, 0.7500000000000001110 ) ;
#1768 = EDGE_CURVE ( 'NONE', #4595, #1560, #1006, .T. ) ;
#1769 = CARTESIAN_POINT ( 'NONE',  ( 3.999956176514755768, 31.00008764698453945, 8.865408859660238505 ) ) ;
#1770 = APPLICATION_PROTOCOL_DEFINITION ( 'draft international standard', 'automotive_design', 1998, #518 ) ;
#1771 = CARTESIAN_POINT ( 'NONE',  ( -23.34254382248203541, 18.84534098761070453, 6.559627254860783019 ) ) ;
#1772 = FACE_OUTER_BOUND ( 'NONE', #4019, .T. ) ;
#1773 = CARTESIAN_POINT ( 'NONE',  ( 26.49999999999999645, -0.5000000000000000000, 19.50000000000000000 ) ) ;
#1774 = ORIENTED_EDGE ( 'NONE', *, *, #3561, .F. ) ;
#1775 = ORIENTED_EDGE ( 'NONE', *, *, #1250, .T. ) ;
#1776 = AXIS2_PLACEMENT_3D ( 'NONE', #1841, #4643, #3947 ) ;
#1777 = FACE_OUTER_BOUND ( 'NONE', #103, .T. ) ;
#1778 = SURFACE_STYLE_USAGE ( .BOTH. , #329 ) ;
#1779 = AXIS2_PLACEMENT_3D ( 'NONE', #38, #1915, #796 ) ;
#1780 = CARTESIAN_POINT ( 'NONE',  ( 0.000000000000000000, 0.000000000000000000, 0.000000000000000000 ) ) ;
#1781 = CARTESIAN_POINT ( 'NONE',  ( -8.000000000000000000, 10.00000000000000178, 17.00000000000000000 ) ) ;
#1782 = EDGE_LOOP ( 'NONE', ( #3974, #4228 ) ) ;
#1783 = DIRECTION ( 'NONE',  ( 0.000000000000000000, 0.000000000000000000, 1.000000000000000000 ) ) ;
#1784 = AXIS2_PLACEMENT_3D ( 'NONE', #3902, #1402, #4698 ) ;
#1785 = FACE_OUTER_BOUND ( 'NONE', #1782, .T. ) ;
#1786 = CARTESIAN_POINT ( 'NONE',  ( 0.7500000000000000000, 0.000000000000000000, 18.19999999999999929 ) ) ;
#1787 = DIRECTION ( 'NONE',  ( 0.000000000000000000, -1.000000000000000000, 0.000000000000000000 ) ) ;
#1788 = ADVANCED_FACE ( 'NONE', ( #2867 ), #4689, .T. ) ;
#1789 = CARTESIAN_POINT ( 'NONE',  ( -25.99307600111999150, -0.5999999999999996447, 19.59999999999999787 ) ) ;
#1790 = EDGE_CURVE ( 'NONE', #2780, #310, #2592, .T. ) ;
#1791 = AXIS2_PLACEMENT_3D ( 'NONE', #3356, #479, #1516 ) ;
#1792 = AXIS2_PLACEMENT_3D ( 'NONE', #874, #2725, #2061 ) ;
#1793 = CARTESIAN_POINT ( 'NONE',  ( 0.000000000000000000, 0.000000000000000000, 20.00000000000000000 ) ) ;
#1794 = APPLICATION_PROTOCOL_DEFINITION ( 'draft international standard', 'automotive_design', 1998, #3923 ) ;
#1795 = CARTESIAN_POINT ( 'NONE',  ( 19.26328748721759609, 22.99914926278827210, 5.984828968106582714 ) ) ;
#1796 = CARTESIAN_POINT ( 'NONE',  ( 4.081770351527290718E-15, 34.00000000000000000, 3.999999999999991562 ) ) ;
#1797 = CARTESIAN_POINT ( 'NONE',  ( -10.25000000000000000, 36.00000000000001421, 2.143131898507868051E-16 ) ) ;
#1798 = ORIENTED_EDGE ( 'NONE', *, *, #2943, .T. ) ;
#1799 = ORIENTED_EDGE ( 'NONE', *, *, #1073, .T. ) ;
#1800 = FACE_OUTER_BOUND ( 'NONE', #1709, .T. ) ;
#1801 =( LENGTH_UNIT ( ) NAMED_UNIT ( * ) SI_UNIT ( .MILLI., .METRE. ) );
#1802 = LINE ( 'NONE', #674, #735 ) ;
#1803 = ORIENTED_EDGE ( 'NONE', *, *, #2251, .F. ) ;
#1804 = EDGE_CURVE ( 'NONE', #1098, #2111, #2453, .T. ) ;
#1805 = ORIENTED_EDGE ( 'NONE', *, *, #2112, .T. ) ;
#1806 = ORIENTED_EDGE ( 'NONE', *, *, #1935, .F. ) ;
#1807 = CIRCLE ( 'NONE', #680, 4.000000000000001776 ) ;
#1808 = DIRECTION ( 'NONE',  ( -1.000000000000000000, -0.000000000000000000, -0.000000000000000000 ) ) ;
#1809 = CARTESIAN_POINT ( 'NONE',  ( 3.606676218660111122, 34.00918236503840575, 7.268492701228249864 ) ) ;
#1810 = VECTOR ( 'NONE', #3966, 1000.000000000000000 ) ;
#1811 = FACE_OUTER_BOUND ( 'NONE', #2919, .T. ) ;
#1812 = VECTOR ( 'NONE', #2741, 1000.000000000000000 ) ;
#1813 = FILL_AREA_STYLE ('',( #4412 ) ) ;
#1814 = CARTESIAN_POINT ( 'NONE',  ( 3.876963039844164793, 31.25679178873219044, 7.985516166298875618 ) ) ;
#1815 = ITEM_DEFINED_TRANSFORMATION ( 'NONE', 'NONE', #662,  #2928 ) ;
#1816 = PRODUCT_DEFINITION ( 'UNKNOWN', '', #1116, #3380 ) ;
#1817 = DIRECTION ( 'NONE',  ( 0.000000000000000000, -0.000000000000000000, 1.000000000000000000 ) ) ;
#1818 = CARTESIAN_POINT ( 'NONE',  ( 3.469446951953614189E-15, 37.00000000000000000, 8.999999999999992895 ) ) ;
#1819 = DIRECTION ( 'NONE',  ( 1.621111868633889227E-15, 1.000000000000000000, 0.000000000000000000 ) ) ;
#1820 = EDGE_LOOP ( 'NONE', ( #556, #2302, #1358, #168 ) ) ;
#1821 = VECTOR ( 'NONE', #1002, 1000.000000000000000 ) ;
#1822 = ORIENTED_EDGE ( 'NONE', *, *, #4059, .F. ) ;
#1823 = FACE_BOUND ( 'NONE', #4209, .T. ) ;
#1824 = SURFACE_SIDE_STYLE ('',( #1488 ) ) ;
#1825 = CARTESIAN_POINT ( 'NONE',  ( -0.5000000000000000000, -0.8660254037844387076, 20.00000000000000000 ) ) ;
#1826 = ORIENTED_EDGE ( 'NONE', *, *, #1399, .F. ) ;
#1827 = ORIENTED_EDGE ( 'NONE', *, *, #974, .T. ) ;
#1828 = EDGE_LOOP ( 'NONE', ( #3877, #4583, #4171, #2177 ) ) ;
#1829 = DIRECTION ( 'NONE',  ( 0.000000000000000000, 1.000000000000000000, 0.000000000000000000 ) ) ;
#1830 = DIRECTION ( 'NONE',  ( 0.000000000000000000, 1.000000000000000000, 0.000000000000000000 ) ) ;
#1831 = FACE_OUTER_BOUND ( 'NONE', #3075, .T. ) ;
#1832 = CARTESIAN_POINT ( 'NONE',  ( -19.58805710660146104, -17.18149551509901940, 20.00001200000000168 ) ) ;
#1833 = VECTOR ( 'NONE', #1711, 1000.000000000000000 ) ;
#1834 = VECTOR ( 'NONE', #3795, 1000.000000000000000 ) ;
#1835 = ORIENTED_EDGE ( 'NONE', *, *, #3330, .F. ) ;
#1836 = PRESENTATION_STYLE_ASSIGNMENT (( #2189 ) ) ;
#1837 = AXIS2_PLACEMENT_3D ( 'NONE', #3841, #2834, #3170 ) ;
#1838 = CARTESIAN_POINT ( 'NONE',  ( 0.000000000000000000, 0.000000000000000000, 18.19999999999999929 ) ) ;
#1839 = CONTEXT_DEPENDENT_SHAPE_REPRESENTATION ( #1481, #2702 ) ;
#1840 = DIRECTION ( 'NONE',  ( -0.000000000000000000, -0.000000000000000000, -1.000000000000000000 ) ) ;
#1841 = CARTESIAN_POINT ( 'NONE',  ( 3.469446951953614189E-15, 37.00000000000000711, 8.999999999999992895 ) ) ;
#1842 = CYLINDRICAL_SURFACE ( 'NONE', #1413, 4.000000000000000000 ) ;
#1843 = ORIENTED_EDGE ( 'NONE', *, *, #2029, .F. ) ;
#1844 = ORIENTED_EDGE ( 'NONE', *, *, #3834, .T. ) ;
#1845 = ADVANCED_FACE ( 'NONE', ( #976 ), #3736, .T. ) ;
#1846 = EDGE_CURVE ( 'NONE', #3324, #477, #1372, .T. ) ;
#1847 = CARTESIAN_POINT ( 'NONE',  ( -0.7500000000000000000, -1.299038105676658450, 17.69999999999999929 ) ) ;
#1848 = CARTESIAN_POINT ( 'NONE',  ( 27.99999999999999645, 3.429011037612588881E-15, 20.00000000000000000 ) ) ;
#1849 = ORIENTED_EDGE ( 'NONE', *, *, #761, .T. ) ;
#1850 = VECTOR ( 'NONE', #4305, 1000.000000000000000 ) ;
#1851 = ORIENTED_EDGE ( 'NONE', *, *, #804, .F. ) ;
#1852 = ORIENTED_EDGE ( 'NONE', *, *, #24, .T. ) ;
#1853 = CARTESIAN_POINT ( 'NONE',  ( 3.469446951953614189E-15, 37.00000000000000000, 8.999999999999992895 ) ) ;
#1854 = CARTESIAN_POINT ( 'NONE',  ( -19.26288713789795537, 22.99946665860929684, 12.01444203287435819 ) ) ;
#1855 = VECTOR ( 'NONE', #1601, 1000.000000000000000 ) ;
#1856 = SURFACE_SIDE_STYLE ('',( #3002 ) ) ;
#1857 = CARTESIAN_POINT ( 'NONE',  ( 23.36965697125208408, -11.52193136556784658, 20.00001200000000168 ) ) ;
#1858 = ORIENTED_EDGE ( 'NONE', *, *, #227, .T. ) ;
#1859 = AXIS2_PLACEMENT_3D ( 'NONE', #1757, #3209, #628 ) ;
#1860 = DIRECTION ( 'NONE',  ( 0.000000000000000000, 0.000000000000000000, -1.000000000000000000 ) ) ;
#1861 = CARTESIAN_POINT ( 'NONE',  ( 8.999999999999980460, 32.99999999999999289, 1.749999999999999778 ) ) ;
#1862 = AXIS2_PLACEMENT_3D ( 'NONE', #4065, #801, #2672 ) ;
#1863 = DIRECTION ( 'NONE',  ( 1.000000000000000000, -0.000000000000000000, 1.224646799147353207E-16 ) ) ;
#1864 = CARTESIAN_POINT ( 'NONE',  ( -3.471149744654747238, 29.79887180468049479, 6.994934987683496530 ) ) ;
#1865 = CARTESIAN_POINT ( 'NONE',  ( -3.464101615137750390, 33.00000000000000000, 10.99999999999999467 ) ) ;
#1866 = AXIS2_PLACEMENT_3D ( 'NONE', #4474, #1287, #1610 ) ;
#1867 = AXIS2_PLACEMENT_3D ( 'NONE', #4432, #2616, #3590 ) ;
#1868 = ORIENTED_EDGE ( 'NONE', *, *, #215, .F. ) ;
#1869 = EDGE_CURVE ( 'NONE', #1336, #1195, #3133, .T. ) ;
#1870 = VERTEX_POINT ( 'NONE', #4038 ) ;
#1871 = EDGE_CURVE ( 'NONE', #1339, #816, #3820, .T. ) ;
#1872 = CARTESIAN_POINT ( 'NONE',  ( 0.000000000000000000, 0.000000000000000000, 19.59999999999999787 ) ) ;
#1873 = DIRECTION ( 'NONE',  ( 0.000000000000000000, 0.000000000000000000, -1.000000000000000000 ) ) ;
#1874 = EDGE_CURVE ( 'NONE', #3472, #3706, #2432, .T. ) ;
#1875 = ORIENTED_EDGE ( 'NONE', *, *, #459, .T. ) ;
#1876 = VERTEX_POINT ( 'NONE', #2574 ) ;
#1877 = VERTEX_POINT ( 'NONE', #366 ) ;
#1878 = ADVANCED_FACE ( 'NONE', ( #1179 ), #732, .F. ) ;
#1879 = UNCERTAINTY_MEASURE_WITH_UNIT (LENGTH_MEASURE( 1.000000000000000082E-05 ), #2838, 'distance_accuracy_value', 'NONE');
#1880 = FACE_OUTER_BOUND ( 'NONE', #4219, .T. ) ;
#1881 = CARTESIAN_POINT ( 'NONE',  ( -27.10000000000000497, 0.6000000000000000888, 19.59999999999999787 ) ) ;
#1882 = SURFACE_STYLE_USAGE ( .BOTH. , #1856 ) ;
#1883 = FACE_OUTER_BOUND ( 'NONE', #4047, .T. ) ;
#1884 = AXIS2_PLACEMENT_3D ( 'NONE', #2691, #4156, #2324 ) ;
#1885 = ORIENTED_EDGE ( 'NONE', *, *, #4427, .T. ) ;
#1886 = DIRECTION ( 'NONE',  ( -0.000000000000000000, 0.000000000000000000, 1.000000000000000000 ) ) ;
#1887 = AXIS2_PLACEMENT_3D ( 'NONE', #3733, #1931, #4103 ) ;
#1888 = DIRECTION ( 'NONE',  ( 0.000000000000000000, 0.000000000000000000, -1.000000000000000000 ) ) ;
#1889=STYLED_ITEM('',(#4729),#2976);
#1890 = CARTESIAN_POINT ( 'NONE',  ( 22.58414294016076695, 19.74853269256671240, 5.528858171306252345 ) ) ;
#1891 = DIRECTION ( 'NONE',  ( -0.000000000000000000, -0.000000000000000000, 1.000000000000000000 ) ) ;
#1892 = SHAPE_REPRESENTATION ( 'reset button', ( #2928 ), #4230 ) ;
#1893 = VECTOR ( 'NONE', #2752, 1000.000000000000000 ) ;
#1894 = DIRECTION ( 'NONE',  ( 8.921435019309286191E-15, 1.000000000000000000, 0.000000000000000000 ) ) ;
#1895 = ORIENTED_EDGE ( 'NONE', *, *, #229, .F. ) ;
#1896 = VERTEX_POINT ( 'NONE', #3604 ) ;
#1897 = EDGE_CURVE ( 'NONE', #4511, #418, #1529, .T. ) ;
#1898 = CARTESIAN_POINT ( 'NONE',  ( 0.5000000000000000000, -2.999999999999999556, 19.50000000000000000 ) ) ;
#1899 = CARTESIAN_POINT ( 'NONE',  ( 3.606497132222534319, 34.00855672170019517, 10.73188315364928513 ) ) ;
#1900 =( NAMED_UNIT ( * ) PLANE_ANGLE_UNIT ( ) SI_UNIT ( $, .RADIAN. ) );
#1901 = CARTESIAN_POINT ( 'NONE',  ( -27.10000000000000497, 0.6000000000000000888, 19.00000000000000000 ) ) ;
#1902 = VERTEX_POINT ( 'NONE', #3315 ) ;
#1903 = ORIENTED_EDGE ( 'NONE', *, *, #2884, .T. ) ;
#1904 = ORIENTED_EDGE ( 'NONE', *, *, #1548, .F. ) ;
#1905 = EDGE_LOOP ( 'NONE', ( #980, #2055, #1141, #3288 ) ) ;
#1906 = DIRECTION ( 'NONE',  ( 0.000000000000000000, 1.000000000000000000, 0.000000000000000000 ) ) ;
#1907 = AXIS2_PLACEMENT_3D ( 'NONE', #147, #2315, #1953 ) ;
#1908 = CARTESIAN_POINT ( 'NONE',  ( -23.60309964903850499, 18.51766120599529231, 10.77116693461329255 ) ) ;
#1909 = CARTESIAN_POINT ( 'NONE',  ( -0.5000000000000001110, 0.000000000000000000, 19.50000000000000000 ) ) ;
#1910 = EDGE_CURVE ( 'NONE', #1928, #3361, #1228, .T. ) ;
#1911 = ORIENTED_EDGE ( 'NONE', *, *, #4685, .F. ) ;
#1912 = EDGE_CURVE ( 'NONE', #3515, #1142, #4208, .T. ) ;
#1913 = DIRECTION ( 'NONE',  ( 0.000000000000000000, 0.000000000000000000, 1.000000000000000000 ) ) ;
#1914 =( GEOMETRIC_REPRESENTATION_CONTEXT ( 3 ) GLOBAL_UNCERTAINTY_ASSIGNED_CONTEXT ( ( #1344 ) ) GLOBAL_UNIT_ASSIGNED_CONTEXT ( ( #1272, #3758, #3450 ) ) REPRESENTATION_CONTEXT ( 'NONE', 'WORKASPACE' ) );
#1915 = DIRECTION ( 'NONE',  ( 0.000000000000000000, 0.000000000000000000, 1.000000000000000000 ) ) ;
#1916 = EDGE_CURVE ( 'NONE', #4308, #499, #1919, .T. ) ;
#1917 = CLOSED_SHELL ( 'NONE', ( #4383, #957, #3287, #2257, #3724, #1415, #4263, #1388, #2101, #2629 ) ) ;
#1918 = VECTOR ( 'NONE', #3458, 1000.000000000000000 ) ;
#1919 = LINE ( 'NONE', #464, #3360 ) ;
#1920 = CARTESIAN_POINT ( 'NONE',  ( -26.00000000000000711, 0.000000000000000000, 20.00000000000000000 ) ) ;
#1921 = CARTESIAN_POINT ( 'NONE',  ( -26.00000000000000355, 0.000000000000000000, 20.00001200000000168 ) ) ;
#1922 = VERTEX_POINT ( 'NONE', #114 ) ;
#1923 = LINE ( 'NONE', #1898, #2655 ) ;
#1924 = DIRECTION ( 'NONE',  ( 1.000000000000000000, 0.000000000000000000, 0.000000000000000000 ) ) ;
#1925 = SURFACE_STYLE_USAGE ( .BOTH. , #2992 ) ;
#1926 = FACE_OUTER_BOUND ( 'NONE', #1097, .T. ) ;
#1927 = ORIENTED_EDGE ( 'NONE', *, *, #751, .T. ) ;
#1928 = VERTEX_POINT ( 'NONE', #2263 ) ;
#1929 = EDGE_LOOP ( 'NONE', ( #2443, #882 ) ) ;
#1930 = VERTEX_POINT ( 'NONE', #3719 ) ;
#1931 = DIRECTION ( 'NONE',  ( 0.000000000000000000, -1.000000000000000000, 0.000000000000000000 ) ) ;
#1932 = CARTESIAN_POINT ( 'NONE',  ( -18.19536891688249014, 23.85222316637480233, 8.999999999999992895 ) ) ;
#1933 =( NAMED_UNIT ( * ) SI_UNIT ( $, .STERADIAN. ) SOLID_ANGLE_UNIT ( ) );
#1934 = ORIENTED_EDGE ( 'NONE', *, *, #2690, .F. ) ;
#1935 = EDGE_CURVE ( 'NONE', #1560, #765, #2953, .T. ) ;
#1936 = AXIS2_PLACEMENT_3D ( 'NONE', #2015, #3468, #2381 ) ;
#1937 = FACE_OUTER_BOUND ( 'NONE', #2766, .T. ) ;
#1938 = CARTESIAN_POINT ( 'NONE',  ( 12.00000000000001954, 44.99999999999999289, 0.000000000000000000 ) ) ;
#1939 = LINE ( 'NONE', #1501, #3753 ) ;
#1940 = TOROIDAL_SURFACE ( 'NONE', #1554, 2.999999999999999112, 1.749999999999999778 ) ;
#1941 = EDGE_CURVE ( 'NONE', #29, #3785, #4129, .T. ) ;
#1942 = ADVANCED_FACE ( 'NONE', ( #381 ), #1761, .T. ) ;
#1943 = CIRCLE ( 'NONE', #1859, 0.9999999999999991118 ) ;
#1944 = DIRECTION ( 'NONE',  ( 1.982541115402063335E-15, 1.000000000000000000, 0.000000000000000000 ) ) ;
#1945 = PLANE ( 'NONE',  #3771 ) ;
#1946 = ORIENTED_EDGE ( 'NONE', *, *, #2540, .F. ) ;
#1947 = AXIS2_PLACEMENT_3D ( 'NONE', #2746, #3509, #617 ) ;
#1948 = DIRECTION ( 'NONE',  ( 0.000000000000000000, -0.7071067811865500152, -0.7071067811865451302 ) ) ;
#1949 = CARTESIAN_POINT ( 'NONE',  ( 3.501826698183293729, 33.52853102779839389, 7.066576927953558851 ) ) ;
#1950 = DIRECTION ( 'NONE',  ( 0.000000000000000000, 0.000000000000000000, 1.000000000000000000 ) ) ;
#1951 = SHAPE_DEFINITION_REPRESENTATION ( #2103, #1892 ) ;
#1952 = CONICAL_SURFACE ( 'NONE', #4535, 5.000000000000000888, 0.7853981633974517207 ) ;
#1953 = DIRECTION ( 'NONE',  ( 1.000000000000000000, 0.000000000000000000, 0.000000000000000000 ) ) ;
#1954 = ORIENTED_EDGE ( 'NONE', *, *, #543, .F. ) ;
#1955 = EDGE_LOOP ( 'NONE', ( #1613, #2019, #1843, #401, #2113 ) ) ;
#1956 = ORIENTED_EDGE ( 'NONE', *, *, #2377, .T. ) ;
#1957 = VERTEX_POINT ( 'NONE', #1197 ) ;
#1958 = ADVANCED_FACE ( 'NONE', ( #3641 ), #2229, .F. ) ;
#1959 = CYLINDRICAL_SURFACE ( 'NONE', #4247, 3.999999999999998224 ) ;
#1960 = UNCERTAINTY_MEASURE_WITH_UNIT (LENGTH_MEASURE( 1.000000000000000082E-05 ), #3300, 'distance_accuracy_value', 'NONE');
#1961 =( LENGTH_UNIT ( ) NAMED_UNIT ( * ) SI_UNIT ( .MILLI., .METRE. ) );
#1962 = DIRECTION ( 'NONE',  ( -0.000000000000000000, -0.000000000000000000, -1.000000000000000000 ) ) ;
#1963 = EDGE_LOOP ( 'NONE', ( #3306, #1934, #1207, #4237 ) ) ;
#1964 = DIRECTION ( 'NONE',  ( 0.000000000000000000, 0.000000000000000000, 1.000000000000000000 ) ) ;
#1965 = CARTESIAN_POINT ( 'NONE',  ( 3.469446951953614189E-15, 25.00000000000000000, 8.999999999999992895 ) ) ;
#1966 = CARTESIAN_POINT ( 'NONE',  ( -12.00000000000000000, 36.00000000000001421, 0.000000000000000000 ) ) ;
#1967 = ORIENTED_EDGE ( 'NONE', *, *, #1561, .T. ) ;
#1968 = VECTOR ( 'NONE', #2952, 1000.000000000000000 ) ;
#1969 = CARTESIAN_POINT ( 'NONE',  ( 18.84548434425194685, 23.34243530581957771, 11.44084376890924304 ) ) ;
#1970 = CARTESIAN_POINT ( 'NONE',  ( 3.469446951953614189E-15, 41.00000000000000000, 3.999999999999990674 ) ) ;
#1971 = EDGE_CURVE ( 'NONE', #1195, #3799, #2208, .T. ) ;
#1972 = TOROIDAL_SURFACE ( 'NONE', #1666, 4.000000000000001776, 1.000000000000000000 ) ;
#1973 = CARTESIAN_POINT ( 'NONE',  ( 3.469446951953614189E-15, 41.00000000000000000, 4.999999999999992006 ) ) ;
#1974 = CARTESIAN_POINT ( 'NONE',  ( 3.522877905629569817, 33.65170801506776854, 10.89542184998092189 ) ) ;
#1975 = DIRECTION ( 'NONE',  ( 0.000000000000000000, 0.000000000000000000, 1.000000000000000000 ) ) ;
#1976 = CARTESIAN_POINT ( 'NONE',  ( 3.469446951953614189E-15, 41.00000000000000000, 8.999999999999992895 ) ) ;
#1977 = ORIENTED_EDGE ( 'NONE', *, *, #1034, .T. ) ;
#1978 = ORIENTED_EDGE ( 'NONE', *, *, #1874, .T. ) ;
#1979 = ORIENTED_EDGE ( 'NONE', *, *, #71, .T. ) ;
#1980 = ORIENTED_EDGE ( 'NONE', *, *, #2095, .F. ) ;
#1981 = DIRECTION ( 'NONE',  ( 0.000000000000000000, 1.000000000000000000, 0.000000000000000000 ) ) ;
#1982 = ORIENTED_EDGE ( 'NONE', *, *, #2540, .T. ) ;
#1983 = AXIS2_PLACEMENT_3D ( 'NONE', #4547, #220, #2049 ) ;
#1984 = LINE ( 'NONE', #2006, #1918 ) ;
#1985 = CARTESIAN_POINT ( 'NONE',  ( 3.469446951953614189E-15, 25.00000000000000000, 8.999999999999992895 ) ) ;
#1986 = DIRECTION ( 'NONE',  ( 0.000000000000000000, 0.000000000000000000, 1.000000000000000000 ) ) ;
#1987 = ORIENTED_EDGE ( 'NONE', *, *, #2862, .F. ) ;
#1988 = PRODUCT_DEFINITION_SHAPE ( 'NONE', 'NONE',  #4712 ) ;
#1989 = CARTESIAN_POINT ( 'NONE',  ( -1.289143957944685281, 29.97326948525437729, 12.79562863665509553 ) ) ;
#1990 = DIRECTION ( 'NONE',  ( -0.000000000000000000, -0.000000000000000000, -1.000000000000000000 ) ) ;
#1991 = CLOSED_SHELL ( 'NONE', ( #3008, #4653, #4700, #3304, #1750, #3991, #3108, #1580, #3130, #1438, #4562, #68, #1362, #1012, #1958, #2897, #3358, #3740, #3863, #3623, #2350, #1100, #2865, #267, #3737, #2562 ) ) ;
#1992 = CARTESIAN_POINT ( 'NONE',  ( -18.21624787168416759, 23.83633674995671470, 8.475268202211100999 ) ) ;
#1993 = DIRECTION ( 'NONE',  ( 0.000000000000000000, 1.000000000000000000, 0.000000000000000000 ) ) ;
#1994 = CARTESIAN_POINT ( 'NONE',  ( 0.000000000000000000, 0.000000000000000000, 20.00001200000000168 ) ) ;
#1995 = ORIENTED_EDGE ( 'NONE', *, *, #3041, .T. ) ;
#1996 = ADVANCED_BREP_SHAPE_REPRESENTATION ( '', ( #3033, #2928 ), #3388 ) ;
#1997 = VERTEX_POINT ( 'NONE', #1881 ) ;
#1998 = ORIENTED_EDGE ( 'NONE', *, *, #2429, .T. ) ;
#1999 = EDGE_CURVE ( 'NONE', #4090, #4401, #2905, .T. ) ;
#2000 = ORIENTED_EDGE ( 'NONE', *, *, #3787, .T. ) ;
#2001 = CARTESIAN_POINT ( 'NONE',  ( 0.000000000000000000, 0.000000000000000000, 18.19999999999999929 ) ) ;
#2002 = EDGE_CURVE ( 'NONE', #906, #3253, #1734, .T. ) ;
#2003 = DIRECTION ( 'NONE',  ( 1.000000000000000000, 0.000000000000000000, -0.000000000000000000 ) ) ;
#2004 = CARTESIAN_POINT ( 'NONE',  ( 0.7500000000000001110, 0.000000000000000000, 17.69999999999999929 ) ) ;
#2005 = ORIENTED_EDGE ( 'NONE', *, *, #611, .T. ) ;
#2006 = CARTESIAN_POINT ( 'NONE',  ( 0.7500000000000001110, 0.000000000000000000, 18.19999999999999929 ) ) ;
#2007 = DIRECTION ( 'NONE',  ( 0.000000000000000000, 1.000000000000000000, 0.000000000000000000 ) ) ;
#2008 = CARTESIAN_POINT ( 'NONE',  ( -0.7500000000000001110, 0.000000000000000000, 15.00000000000000178 ) ) ;
#2009 = ORIENTED_EDGE ( 'NONE', *, *, #3700, .T. ) ;
#2010 = CIRCLE ( 'NONE', #3076, 5.500000000000000000 ) ;
#2011 = CARTESIAN_POINT ( 'NONE',  ( 19.92007681871562497, 22.43321928693944400, 12.59316242105108685 ) ) ;
#2012 = LINE ( 'NONE', #3111, #4461 ) ;
#2013 = CIRCLE ( 'NONE', #729, 0.7500000000000001110 ) ;
#2014 = DIRECTION ( 'NONE',  ( -0.000000000000000000, -0.000000000000000000, 1.000000000000000000 ) ) ;
#2015 = CARTESIAN_POINT ( 'NONE',  ( 3.889087296525981063, 37.00000000000000000, 12.88908729652603746 ) ) ;
#2016 = DIRECTION ( 'NONE',  ( 0.000000000000000000, 0.000000000000000000, 1.000000000000000000 ) ) ;
#2017 = LINE ( 'NONE', #2361, #527 ) ;
#2018 = ORIENTED_EDGE ( 'NONE', *, *, #2084, .F. ) ;
#2019 = ORIENTED_EDGE ( 'NONE', *, *, #897, .F. ) ;
#2020 = EDGE_LOOP ( 'NONE', ( #3493, #4114, #148, #4203 ) ) ;
#2021 = EDGE_CURVE ( 'NONE', #3729, #85, #2144, .T. ) ;
#2022 = VERTEX_POINT ( 'NONE', #3024 ) ;
#2023 = CARTESIAN_POINT ( 'NONE',  ( 3.469446951953614189E-15, 39.99999999999999289, 3.999999999999991562 ) ) ;
#2024 = PRESENTATION_LAYER_ASSIGNMENT (  '', '', ( #3921 ) ) ;
#2025 = DIRECTION ( 'NONE',  ( -1.000000000000000000, -0.000000000000000000, -0.000000000000000000 ) ) ;
#2026 = CIRCLE ( 'NONE', #3850, 0.7500000000000001110 ) ;
#2027 = EDGE_CURVE ( 'NONE', #2482, #181, #57, .T. ) ;
#2028 = DIRECTION ( 'NONE',  ( -1.000000000000000000, 0.000000000000000000, 0.000000000000000000 ) ) ;
#2029 = EDGE_CURVE ( 'NONE', #2036, #1997, #3100, .T. ) ;
#2030 = VERTEX_POINT ( 'NONE', #1224 ) ;
#2031 = PRODUCT ( 'ring', 'ring', '', ( #684 ) ) ;
#2032 = CARTESIAN_POINT ( 'NONE',  ( 3.469446951953614189E-15, 37.00000000000000711, 4.999999999999992006 ) ) ;
#2033 = PRODUCT_DEFINITION_FORMATION_WITH_SPECIFIED_SOURCE ( 'ANY', '', #2787, .NOT_KNOWN. ) ;
#2034 = DIRECTION ( 'NONE',  ( 0.000000000000000000, 0.000000000000000000, -1.000000000000000000 ) ) ;
#2035 = CARTESIAN_POINT ( 'NONE',  ( 3.469446951953614189E-15, 41.00000000000000000, 8.999999999999992895 ) ) ;
#2036 = VERTEX_POINT ( 'NONE', #817 ) ;
#2037 = CARTESIAN_POINT ( 'NONE',  ( -2.642157743709451889, 29.88401080970086099, 12.01472878375391140 ) ) ;
#2038 = CARTESIAN_POINT ( 'NONE',  ( 27.09999999999999787, 0.6000000000000000888, 19.59999999999999787 ) ) ;
#2039 = CIRCLE ( 'NONE', #4093, 24.00000000000000355 ) ;
#2040 = CARTESIAN_POINT ( 'NONE',  ( -21.93550942649232383, 20.46703030200853135, 5.128274502689557757 ) ) ;
#2041 = AXIS2_PLACEMENT_3D ( 'NONE', #4358, #1101, #56 ) ;
#2042 = PLANE ( 'NONE',  #2947 ) ;
#2043 = DIRECTION ( 'NONE',  ( 0.000000000000000000, 0.000000000000000000, 1.000000000000000000 ) ) ;
#2044 = VERTEX_POINT ( 'NONE', #1252 ) ;
#2045 = ORIENTED_EDGE ( 'NONE', *, *, #4098, .T. ) ;
#2046 = ORIENTED_EDGE ( 'NONE', *, *, #916, .F. ) ;
#2047 = CIRCLE ( 'NONE', #682, 26.00000000000000711 ) ;
#2048 = DIRECTION ( 'NONE',  ( -0.000000000000000000, -0.000000000000000000, -1.000000000000000000 ) ) ;
#2049 = DIRECTION ( 'NONE',  ( -1.000000000000000000, 0.000000000000000000, 0.000000000000000000 ) ) ;
#2050 = CARTESIAN_POINT ( 'NONE',  ( 0.000000000000000000, 10.00000000000000000, 13.00000000000000178 ) ) ;
#2051 = DIRECTION ( 'NONE',  ( -0.7071067811865437980, 0.000000000000000000, -0.7071067811865512365 ) ) ;
#2052 = CARTESIAN_POINT ( 'NONE',  ( -8.999999999999973355, 32.99999999999999289, 0.000000000000000000 ) ) ;
#2053 = DIRECTION ( 'NONE',  ( 0.000000000000000000, 0.000000000000000000, -1.000000000000000000 ) ) ;
#2054 = EDGE_CURVE ( 'NONE', #2878, #1270, #2643, .T. ) ;
#2055 = ORIENTED_EDGE ( 'NONE', *, *, #4488, .F. ) ;
#2056 = VECTOR ( 'NONE', #2014, 1000.000000000000000 ) ;
#2057 = EDGE_CURVE ( 'NONE', #1507, #1896, #2282, .T. ) ;
#2058 = EDGE_CURVE ( 'NONE', #52, #3445, #631, .T. ) ;
#2059 = SURFACE_STYLE_USAGE ( .BOTH. , #2444 ) ;
#2060 = DIRECTION ( 'NONE',  ( -1.000000000000000000, 0.000000000000000000, -0.000000000000000000 ) ) ;
#2061 = DIRECTION ( 'NONE',  ( -1.000000000000000000, 0.000000000000000000, -3.469446951953614189E-15 ) ) ;
#2062 = CARTESIAN_POINT ( 'NONE',  ( -26.50000000000000355, -0.5000000000000000000, 19.00000000000000000 ) ) ;
#2063 = DIRECTION ( 'NONE',  ( -0.000000000000000000, -1.000000000000000000, -0.000000000000000000 ) ) ;
#2064 = PRODUCT ( 'reset button', 'reset button', '', ( #1134 ) ) ;
#2065 = CARTESIAN_POINT ( 'NONE',  ( -25.83240171513484640, 3.403349963601426165, 20.00001199999999812 ) ) ;
#2066 = AXIS2_PLACEMENT_3D ( 'NONE', #1355, #4590, #3894 ) ;
#2067 = ORIENTED_EDGE ( 'NONE', *, *, #3106, .T. ) ;
#2068 = EDGE_LOOP ( 'NONE', ( #1826, #2219, #2281, #4645 ) ) ;
#2069 = CYLINDRICAL_SURFACE ( 'NONE', #4016, 0.7500000000000001110 ) ;
#2070 = AXIS2_PLACEMENT_3D ( 'NONE', #2174, #1817, #1113 ) ;
#2071 =( NAMED_UNIT ( * ) PLANE_ANGLE_UNIT ( ) SI_UNIT ( $, .RADIAN. ) );
#2072 = DIRECTION ( 'NONE',  ( 0.000000000000000000, 1.000000000000000000, 0.000000000000000000 ) ) ;
#2073 = CARTESIAN_POINT ( 'NONE',  ( 6.741346781237198549, 25.16843286583315020, 20.00001200000000168 ) ) ;
#2074 = DIRECTION ( 'NONE',  ( -1.000000000000000000, 0.000000000000000000, 0.000000000000000000 ) ) ;
#2075 = FACE_OUTER_BOUND ( 'NONE', #1905, .T. ) ;
#2076 = DIRECTION ( 'NONE',  ( 0.000000000000000000, -1.000000000000000000, 0.000000000000000000 ) ) ;
#2077 = ORIENTED_EDGE ( 'NONE', *, *, #2217, .T. ) ;
#2078 = EDGE_CURVE ( 'NONE', #3924, #127, #3028, .T. ) ;
#2079 = LINE ( 'NONE', #2401, #3946 ) ;
#2080 = CARTESIAN_POINT ( 'NONE',  ( -0.7500000000000000000, 0.000000000000000000, 18.19999999999999929 ) ) ;
#2081 = VECTOR ( 'NONE', #3154, 1000.000000000000000 ) ;
#2082 = CARTESIAN_POINT ( 'NONE',  ( 1.701696020694480449, -26.00000000000000355, 20.00001200000000878 ) ) ;
#2083 = EDGE_CURVE ( 'NONE', #3353, #3204, #892, .T. ) ;
#2084 = EDGE_CURVE ( 'NONE', #1876, #2731, #3077, .T. ) ;
#2085 = VECTOR ( 'NONE', #3079, 1000.000000000000000 ) ;
#2086 = DIRECTION ( 'NONE',  ( 0.000000000000000000, 0.000000000000000000, 1.000000000000000000 ) ) ;
#2087 = DIRECTION ( 'NONE',  ( 1.000000000000000000, 0.000000000000000000, 1.040834085586084257E-14 ) ) ;
#2088 = DIRECTION ( 'NONE',  ( 0.000000000000000000, 0.000000000000000000, 1.000000000000000000 ) ) ;
#2089 = COLOUR_RGB ( '',0.8941176470588234615, 0.8941176470588234615, 0.8941176470588234615 ) ;
#2090 = VERTEX_POINT ( 'NONE', #1577 ) ;
#2091 = VERTEX_POINT ( 'NONE', #558 ) ;
#2092 = DIRECTION ( 'NONE',  ( 0.000000000000000000, 0.000000000000000000, 1.000000000000000000 ) ) ;
#2093 = EDGE_LOOP ( 'NONE', ( #4291, #3164 ) ) ;
#2094 = CARTESIAN_POINT ( 'NONE',  ( -0.9958591954639911537, 37.00000000000000000, 14.40909090909089052 ) ) ;
#2095 = EDGE_CURVE ( 'NONE', #499, #2636, #4508, .T. ) ;
#2096 = COLOUR_RGB ( '',0.8941176470588234615, 0.8941176470588234615, 0.8941176470588234615 ) ;
#2097 = AXIS2_PLACEMENT_3D ( 'NONE', #303, #4669, #3948 ) ;
#2098 = CARTESIAN_POINT ( 'NONE',  ( 3.469446951953614189E-15, 25.00000000000000000, 4.999999999999992006 ) ) ;
#2099 = FACE_OUTER_BOUND ( 'NONE', #3630, .T. ) ;
#2100 = CARTESIAN_POINT ( 'NONE',  ( 3.470161297262016831, 29.79898158544631670, 11.00652372288853975 ) ) ;
#2101 = ADVANCED_FACE ( 'NONE', ( #201 ), #3972, .T. ) ;
#2102 = CIRCLE ( 'NONE', #663, 4.000000000000000000 ) ;
#2103 = PRODUCT_DEFINITION_SHAPE ( 'NONE', 'NONE',  #1555 ) ;
#2104 = CARTESIAN_POINT ( 'NONE',  ( 23.60157000768436930, 18.51961241432701399, 10.77614164618340631 ) ) ;
#2105 = DIRECTION ( 'NONE',  ( -0.000000000000000000, -0.000000000000000000, -1.000000000000000000 ) ) ;
#2106 = CARTESIAN_POINT ( 'NONE',  ( -22.43020886076084253, 19.92346879083515176, 5.404597446377701786 ) ) ;
#2107 = DIRECTION ( 'NONE',  ( 8.659560562354962440E-17, 0.7071067811865451302, -0.7071067811865500152 ) ) ;
#2108 = AXIS2_PLACEMENT_3D ( 'NONE', #446, #1538, #2991 ) ;
#2109 = CARTESIAN_POINT ( 'NONE',  ( 11.99999999999999822, 45.00000000000000000, 0.000000000000000000 ) ) ;
#2110 = EDGE_CURVE ( 'NONE', #765, #1270, #1984, .T. ) ;
#2111 = VERTEX_POINT ( 'NONE', #157 ) ;
#2112 = EDGE_CURVE ( 'NONE', #1468, #2610, #1552, .T. ) ;
#2113 = ORIENTED_EDGE ( 'NONE', *, *, #1035, .F. ) ;
#2114 = VECTOR ( 'NONE', #1592, 1000.000000000000000 ) ;
#2115 = DIRECTION ( 'NONE',  ( 0.000000000000000000, 0.000000000000000000, -1.000000000000000000 ) ) ;
#2116 = DIRECTION ( 'NONE',  ( -0.000000000000000000, -0.000000000000000000, -1.000000000000000000 ) ) ;
#2117 = DIRECTION ( 'NONE',  ( -0.000000000000000000, -1.000000000000000000, -0.000000000000000000 ) ) ;
#2118 = CIRCLE ( 'NONE', #1135, 30.00000000000000355 ) ;
#2119 = AXIS2_PLACEMENT_3D ( 'NONE', #4251, #4684, #1328 ) ;
#2120 = VERTEX_POINT ( 'NONE', #3716 ) ;
#2121 = CARTESIAN_POINT ( 'NONE',  ( 30.00000000000000355, 3.673940397442059967E-15, 0.000000000000000000 ) ) ;
#2122 = FACE_OUTER_BOUND ( 'NONE', #931, .T. ) ;
#2123 = CIRCLE ( 'NONE', #4319, 0.7500000000000001110 ) ;
#2124 = LINE ( 'NONE', #3570, #1139 ) ;
#2125 = CARTESIAN_POINT ( 'NONE',  ( 0.5260335297454653558, 29.99650222249029952, 5.025987840185457856 ) ) ;
#2126 = FILL_AREA_STYLE ('',( #3548 ) ) ;
#2127 = CARTESIAN_POINT ( 'NONE',  ( 3.948082828799474697, 31.10544434314014239, 8.346052798592717537 ) ) ;
#2128 = APPLICATION_PROTOCOL_DEFINITION ( 'draft international standard', 'automotive_design', 1998, #2795 ) ;
#2129 = CARTESIAN_POINT ( 'NONE',  ( -20.67279826512042007, -15.85973458909327150, 20.00001200000000168 ) ) ;
#2130 = AXIS2_PLACEMENT_3D ( 'NONE', #3371, #523, #497 ) ;
#2131 = CARTESIAN_POINT ( 'NONE',  ( 0.000000000000000000, 0.000000000000000000, 19.50000000000000000 ) ) ;
#2132 = CARTESIAN_POINT ( 'NONE',  ( 4.081770351527290718E-15, 34.00000000000000000, 13.99999999999999289 ) ) ;
#2133 = CARTESIAN_POINT ( 'NONE',  ( 2.255140518769849223E-14, 49.00000000000000000, 4.499999999999992895 ) ) ;
#2134 = ORIENTED_EDGE ( 'NONE', *, *, #4326, .F. ) ;
#2135 = VERTEX_POINT ( 'NONE', #3005 ) ;
#2136 = AXIS2_PLACEMENT_3D ( 'NONE', #4421, #2606, #926 ) ;
#2137 = FILL_AREA_STYLE ('',( #4624 ) ) ;
#2138 = DIRECTION ( 'NONE',  ( 1.000000000000000000, 0.000000000000000000, 0.000000000000000000 ) ) ;
#2139 = EDGE_CURVE ( 'NONE', #1375, #4484, #176, .T. ) ;
#2140 = ORIENTED_EDGE ( 'NONE', *, *, #924, .T. ) ;
#2141 = CARTESIAN_POINT ( 'NONE',  ( 26.00000000000000711, 1.701696020694481559, 20.00001200000000523 ) ) ;
#2142 = EDGE_CURVE ( 'NONE', #3119, #52, #178, .T. ) ;
#2143 = CLOSED_SHELL ( 'NONE', ( #820, #562, #3805, #2749, #113, #386, #1526, #3104, #1059, #2895, #3414, #2984, #3887, #1670 ) ) ;
#2144 = CIRCLE ( 'NONE', #3510, 5.000000000000000888 ) ;
#2145 = LINE ( 'NONE', #402, #3166 ) ;
#2146 = DIRECTION ( 'NONE',  ( 0.000000000000000000, 0.000000000000000000, 1.000000000000000000 ) ) ;
#2147 = CARTESIAN_POINT ( 'NONE',  ( 2.440861994934926837, 29.90134041232742490, 12.17981090101949349 ) ) ;
#2148 = DIRECTION ( 'NONE',  ( -1.000000000000000000, 0.000000000000000000, 0.000000000000000000 ) ) ;
#2149 = DIRECTION ( 'NONE',  ( 0.000000000000000000, 0.000000000000000000, -1.000000000000000000 ) ) ;
#2150 = ITEM_DEFINED_TRANSFORMATION ( 'NONE', 'NONE', #3853,  #2928 ) ;
#2151 = DIRECTION ( 'NONE',  ( 0.000000000000000000, 0.000000000000000000, -1.000000000000000000 ) ) ;
#2152 = EDGE_CURVE ( 'NONE', #3697, #1485, #1623, .T. ) ;
#2153 = CARTESIAN_POINT ( 'NONE',  ( 0.000000000000000000, 20.00000000000000000, 18.19999999999999929 ) ) ;
#2154 = CARTESIAN_POINT ( 'NONE',  ( -3.464101615137750390, 33.00000000000000000, 6.999999999999991118 ) ) ;
#2155 = ORIENTED_EDGE ( 'NONE', *, *, #2586, .T. ) ;
#2156 = ORIENTED_EDGE ( 'NONE', *, *, #2755, .F. ) ;
#2157 = VECTOR ( 'NONE', #4063, 1000.000000000000000 ) ;
#2158 = CARTESIAN_POINT ( 'NONE',  ( 0.000000000000000000, 0.000000000000000000, 19.00000000000000000 ) ) ;
#2159 = SURFACE_STYLE_FILL_AREA ( #2137 ) ;
#2160 = CARTESIAN_POINT ( 'NONE',  ( 3.469446951953614189E-15, 37.00000000000000000, 8.999999999999992895 ) ) ;
#2161 = ORIENTED_EDGE ( 'NONE', *, *, #1703, .F. ) ;
#2162 = ORIENTED_EDGE ( 'NONE', *, *, #749, .T. ) ;
#2163 = CARTESIAN_POINT ( 'NONE',  ( -1.701696020694479783, 25.99999999999999645, 20.00001200000000523 ) ) ;
#2164 = AXIS2_PLACEMENT_3D ( 'NONE', #4030, #770, #2206 ) ;
#2165 = DIRECTION ( 'NONE',  ( 0.7071067811865487940, 0.7071067811865463515, -0.000000000000000000 ) ) ;
#2166 = DIRECTION ( 'NONE',  ( -1.000000000000000000, 0.000000000000000000, 0.000000000000000000 ) ) ;
#2167 = DIRECTION ( 'NONE',  ( 0.000000000000000000, 0.000000000000000000, -1.000000000000000000 ) ) ;
#2168 = ADVANCED_FACE ( 'NONE', ( #1276 ), #2716, .T. ) ;
#2169 = AXIS2_PLACEMENT_3D ( 'NONE', #1994, #2802, #3808 ) ;
#2170 = SURFACE_STYLE_FILL_AREA ( #1813 ) ;
#2171 = AXIS2_PLACEMENT_3D ( 'NONE', #1140, #4441, #466 ) ;
#2172 = FACE_OUTER_BOUND ( 'NONE', #4701, .T. ) ;
#2173 = CONTEXT_DEPENDENT_SHAPE_REPRESENTATION ( #3251, #4163 ) ;
#2174 = CARTESIAN_POINT ( 'NONE',  ( 0.000000000000000000, 0.000000000000000000, 19.50000000000000000 ) ) ;
#2175 = LINE ( 'NONE', #2504, #3837 ) ;
#2176 = DIRECTION ( 'NONE',  ( 0.000000000000000000, -1.000000000000000000, -0.000000000000000000 ) ) ;
#2177 = ORIENTED_EDGE ( 'NONE', *, *, #2861, .F. ) ;
#2178 = ORIENTED_EDGE ( 'NONE', *, *, #1440, .T. ) ;
#2179 = CARTESIAN_POINT ( 'NONE',  ( -3.971780439164231513, 31.05502319471607819, 9.533653685786568133 ) ) ;
#2180 = DIRECTION ( 'NONE',  ( 0.000000000000000000, 1.000000000000000000, 0.000000000000000000 ) ) ;
#2181 = EDGE_LOOP ( 'NONE', ( #426, #3756, #3738, #4433 ) ) ;
#2182 = ORIENTED_EDGE ( 'NONE', *, *, #2884, .F. ) ;
#2183 = ORIENTED_EDGE ( 'NONE', *, *, #2475, .T. ) ;
#2184 = AXIS2_PLACEMENT_3D ( 'NONE', #1429, #2165, #3237 ) ;
#2185 = DIRECTION ( 'NONE',  ( -0.000000000000000000, -1.000000000000000000, -0.000000000000000000 ) ) ;
#2186 = CARTESIAN_POINT ( 'NONE',  ( -23.72657184721640533, 18.35919055844626158, 10.28976100101469981 ) ) ;
#2187 = ORIENTED_EDGE ( 'NONE', *, *, #2781, .T. ) ;
#2188 = VECTOR ( 'NONE', #3101, 1000.000000000000000 ) ;
#2189 = SURFACE_STYLE_USAGE ( .BOTH. , #748 ) ;
#2190 = DIRECTION ( 'NONE',  ( 0.000000000000000000, 1.000000000000000000, 0.000000000000000000 ) ) ;
#2191 = EDGE_CURVE ( 'NONE', #742, #1614, #4665, .T. ) ;
#2192 = ADVANCED_FACE ( 'NONE', ( #1937 ), #3385, .T. ) ;
#2193 = CARTESIAN_POINT ( 'NONE',  ( 3.889087296526035242, 37.00000000000000000, 5.110912703473999841 ) ) ;
#2194 = CARTESIAN_POINT ( 'NONE',  ( -25.99307600111999150, -0.5999999999999998668, 20.00001200000000168 ) ) ;
#2195 = CARTESIAN_POINT ( 'NONE',  ( -3.522982843720154467, 33.65196231893016687, 10.89519766348715457 ) ) ;
#2196 = VERTEX_POINT ( 'NONE', #966 ) ;
#2197 = VECTOR ( 'NONE', #4423, 1000.000000000000000 ) ;
#2198 = ORIENTED_EDGE ( 'NONE', *, *, #3857, .T. ) ;
#2199 = DIRECTION ( 'NONE',  ( 0.000000000000000000, 0.000000000000000000, 1.000000000000000000 ) ) ;
#2200 = LINE ( 'NONE', #1848, #698 ) ;
#2201 = ORIENTED_EDGE ( 'NONE', *, *, #4620, .T. ) ;
#2202 = ORIENTED_EDGE ( 'NONE', *, *, #1790, .T. ) ;
#2203 = ORIENTED_EDGE ( 'NONE', *, *, #3618, .T. ) ;
#2204 = LINE ( 'NONE', #1493, #1968 ) ;
#2205 = CARTESIAN_POINT ( 'NONE',  ( -18.97751144565075165, 23.23549755865085231, 11.64625228532891121 ) ) ;
#2206 = DIRECTION ( 'NONE',  ( -1.000000000000000000, 0.000000000000000000, 0.000000000000000000 ) ) ;
#2207 = CARTESIAN_POINT ( 'NONE',  ( 17.18149551509901585, -19.58805710660145749, 20.00001200000000168 ) ) ;
#2208 = CIRCLE ( 'NONE', #387, 5.000000000000002665 ) ;
#2209 = ORIENTED_EDGE ( 'NONE', *, *, #3457, .T. ) ;
#2210 =( NAMED_UNIT ( * ) PLANE_ANGLE_UNIT ( ) SI_UNIT ( $, .RADIAN. ) );
#2211 = CIRCLE ( 'NONE', #2829, 1.000000000000000000 ) ;
#2212 = PLANE ( 'NONE',  #3222 ) ;
#2213 = EDGE_CURVE ( 'NONE', #763, #1192, #782, .T. ) ;
#2214 = EDGE_CURVE ( 'NONE', #4100, #4120, #1767, .T. ) ;
#2215 = CARTESIAN_POINT ( 'NONE',  ( 23.52555220673924197, 18.61638332444494992, 6.995423750305945987 ) ) ;
#2216 = CARTESIAN_POINT ( 'NONE',  ( -3.178742173564956808, 29.83148068024111410, 6.557713274934318548 ) ) ;
#2217 = EDGE_CURVE ( 'NONE', #1290, #954, #2211, .T. ) ;
#2218 = CARTESIAN_POINT ( 'NONE',  ( 3.469446951953614189E-15, 41.00000000000000000, 8.999999999999992895 ) ) ;
#2219 = ORIENTED_EDGE ( 'NONE', *, *, #1731, .T. ) ;
#2220 = ORIENTED_EDGE ( 'NONE', *, *, #2538, .F. ) ;
#2221 = CARTESIAN_POINT ( 'NONE',  ( -3.501826698183285735, 32.47146897220161321, 7.066576927953555298 ) ) ;
#2222 = PRESENTATION_STYLE_ASSIGNMENT (( #1925 ) ) ;
#2223 = CARTESIAN_POINT ( 'NONE',  ( 3.469446951953614189E-15, 40.00000000000000000, 8.999999999999992895 ) ) ;
#2224 = ORIENTED_EDGE ( 'NONE', *, *, #2866, .F. ) ;
#2225 = AXIS2_PLACEMENT_3D ( 'NONE', #4668, #2523, #3992 ) ;
#2226 = ORIENTED_EDGE ( 'NONE', *, *, #2569, .T. ) ;
#2227 = ORIENTED_EDGE ( 'NONE', *, *, #1700, .T. ) ;
#2228 = LINE ( 'NONE', #3261, #3792 ) ;
#2229 = PLANE ( 'NONE',  #20 ) ;
#2230 = VECTOR ( 'NONE', #3172, 1000.000000000000000 ) ;
#2231 = CARTESIAN_POINT ( 'NONE',  ( 0.000000000000000000, 0.000000000000000000, 18.19999999999999929 ) ) ;
#2232 = CARTESIAN_POINT ( 'NONE',  ( -24.67207871933483432, -8.377607117416806304, 20.00001200000000168 ) ) ;
#2233 = ORIENTED_EDGE ( 'NONE', *, *, #4105, .F. ) ;
#2234 = CIRCLE ( 'NONE', #2848, 1.500000000000000222 ) ;
#2235 = SURFACE_SIDE_STYLE ('',( #2170 ) ) ;
#2236 = EDGE_CURVE ( 'NONE', #906, #3494, #3124, .T. ) ;
#2237 = CARTESIAN_POINT ( 'NONE',  ( 3.672134815396417284, 31.76998607164104627, 10.59780778022629200 ) ) ;
#2238 = EDGE_CURVE ( 'NONE', #2608, #2276, #4654, .T. ) ;
#2239 = CIRCLE ( 'NONE', #4693, 1.000000000000000888 ) ;
#2240 = DIRECTION ( 'NONE',  ( 1.000000000000000000, 0.000000000000000000, 0.000000000000000000 ) ) ;
#2241 = CARTESIAN_POINT ( 'NONE',  ( -8.999999999999973355, 32.99999999999999289, -1.749999999999999778 ) ) ;
#2242 = CARTESIAN_POINT ( 'NONE',  ( 8.999999999999980460, 32.99999999999999289, 0.000000000000000000 ) ) ;
#2243 = PRODUCT_DEFINITION_FORMATION_WITH_SPECIFIED_SOURCE ( 'ANY', '', #206, .NOT_KNOWN. ) ;
#2244 = ORIENTED_EDGE ( 'NONE', *, *, #1971, .T. ) ;
#2245 = EDGE_LOOP ( 'NONE', ( #533, #394, #151, #3056 ) ) ;
#2246 = DIRECTION ( 'NONE',  ( 0.000000000000000000, 0.000000000000000000, -1.000000000000000000 ) ) ;
#2247 = CARTESIAN_POINT ( 'NONE',  ( 3.707290417464801813, 34.32328140140740658, 10.50513240900691336 ) ) ;
#2248 = PRODUCT_DEFINITION ( 'UNKNOWN', '', #4003, #2279 ) ;
#2249 = LINE ( 'NONE', #832, #2197 ) ;
#2250 = ORIENTED_EDGE ( 'NONE', *, *, #363, .T. ) ;
#2251 = EDGE_CURVE ( 'NONE', #3492, #1168, #608, .T. ) ;
#2252 = ORIENTED_EDGE ( 'NONE', *, *, #2238, .F. ) ;
#2253 = ORIENTED_EDGE ( 'NONE', *, *, #2054, .F. ) ;
#2254 = UNCERTAINTY_MEASURE_WITH_UNIT (LENGTH_MEASURE( 1.000000000000000082E-05 ), #1642, 'distance_accuracy_value', 'NONE');
#2255 = LINE ( 'NONE', #1196, #2114 ) ;
#2256 = CARTESIAN_POINT ( 'NONE',  ( -19.42075468095228530, 22.86660962422639898, 12.18297904795690378 ) ) ;
#2257 = ADVANCED_FACE ( 'NONE', ( #1715 ), #2739, .T. ) ;
#2258 = ORIENTED_EDGE ( 'NONE', *, *, #2392, .T. ) ;
#2259 = CARTESIAN_POINT ( 'NONE',  ( 3.469446951953614189E-15, 37.00000000000000000, 8.999999999999992895 ) ) ;
#2260 = CIRCLE ( 'NONE', #222, 5.500000000000000000 ) ;
#2261 = CARTESIAN_POINT ( 'NONE',  ( 0.7500000000000000000, -2.999999999999999556, 17.69999999999999929 ) ) ;
#2262 = AXIS2_PLACEMENT_3D ( 'NONE', #1697, #3573, #316 ) ;
#2263 = CARTESIAN_POINT ( 'NONE',  ( 23.85222316637486273, 18.19536891688240843, 8.999999999999992895 ) ) ;
#2264 = CARTESIAN_POINT ( 'NONE',  ( -2.439210544738880326, 29.90146712018378494, 5.819033386899011617 ) ) ;
#2265 = CYLINDRICAL_SURFACE ( 'NONE', #2857, 1.500000000000000222 ) ;
#2266 = ORIENTED_EDGE ( 'NONE', *, *, #4287, .F. ) ;
#2267 = CARTESIAN_POINT ( 'NONE',  ( -3.877033663942010211, 31.25660811682476492, 7.985269980068073536 ) ) ;
#2268 = CARTESIAN_POINT ( 'NONE',  ( 3.472015849686738598, 33.26730327278065147, 10.98645679572690348 ) ) ;
#2269 =( NAMED_UNIT ( * ) PLANE_ANGLE_UNIT ( ) SI_UNIT ( $, .RADIAN. ) );
#2270 = DIRECTION ( 'NONE',  ( 0.000000000000000000, 1.000000000000000000, 0.000000000000000000 ) ) ;
#2271 = EDGE_LOOP ( 'NONE', ( #2202, #3045, #4249, #2708 ) ) ;
#2272 = EDGE_CURVE ( 'NONE', #418, #1588, #4245, .T. ) ;
#2273 = CIRCLE ( 'NONE', #4123, 0.7500000000000001110 ) ;
#2274 = ORIENTED_EDGE ( 'NONE', *, *, #2392, .F. ) ;
#2275 = ORIENTED_EDGE ( 'NONE', *, *, #3531, .F. ) ;
#2276 = VERTEX_POINT ( 'NONE', #2098 ) ;
#2277 = FACE_OUTER_BOUND ( 'NONE', #3350, .T. ) ;
#2278 = CARTESIAN_POINT ( 'NONE',  ( -22.86919556969945333, 19.41770456673549106, 12.17989986600643348 ) ) ;
#2279 = PRODUCT_DEFINITION_CONTEXT ( 'detailed design', #518, 'design' ) ;
#2280 = ADVANCED_FACE ( 'NONE', ( #2122 ), #3545, .T. ) ;
#2281 = ORIENTED_EDGE ( 'NONE', *, *, #1040, .T. ) ;
#2282 = LINE ( 'NONE', #2689, #1318 ) ;
#2283 = CIRCLE ( 'NONE', #3355, 26.00000000000000711 ) ;
#2284 = DIRECTION ( 'NONE',  ( 0.000000000000000000, 1.000000000000000000, 0.000000000000000000 ) ) ;
#2285 = AXIS2_PLACEMENT_3D ( 'NONE', #346, #4344, #4367 ) ;
#2286 = CARTESIAN_POINT ( 'NONE',  ( -0.5247320085691752345, 29.99650235037416834, 5.025996973432255821 ) ) ;
#2287 = CYLINDRICAL_SURFACE ( 'NONE', #3998, 30.00000000000000355 ) ;
#2288 = VERTEX_POINT ( 'NONE', #3569 ) ;
#2289 = ADVANCED_FACE ( 'NONE', ( #1763 ), #1031, .F. ) ;
#2290 = DIRECTION ( 'NONE',  ( 0.000000000000000000, -0.000000000000000000, 1.000000000000000000 ) ) ;
#2291 = CARTESIAN_POINT ( 'NONE',  ( 3.948598437009898987, 34.89563602083902794, 8.348972239903947212 ) ) ;
#2292 = DIRECTION ( 'NONE',  ( 1.000000000000000000, 0.000000000000000000, 0.000000000000000000 ) ) ;
#2293 = DIRECTION ( 'NONE',  ( -0.000000000000000000, -1.000000000000000000, -0.000000000000000000 ) ) ;
#2294 = EDGE_LOOP ( 'NONE', ( #3003, #772, #1052, #3609 ) ) ;
#2295 = ORIENTED_EDGE ( 'NONE', *, *, #1386, .F. ) ;
#2296 = VERTEX_POINT ( 'NONE', #4225 ) ;
#2297 = VERTEX_POINT ( 'NONE', #3935 ) ;
#2298 = DIRECTION ( 'NONE',  ( -1.734723475976807094E-15, 0.000000000000000000, 1.000000000000000000 ) ) ;
#2299 = CARTESIAN_POINT ( 'NONE',  ( 0.000000000000000000, 0.000000000000000000, 19.00000000000000000 ) ) ;
#2300 = VECTOR ( 'NONE', #1088, 1000.000000000000000 ) ;
#2301 = DIRECTION ( 'NONE',  ( -0.000000000000000000, -1.000000000000000000, -0.000000000000000000 ) ) ;
#2302 = ORIENTED_EDGE ( 'NONE', *, *, #3086, .F. ) ;
#2303 = CARTESIAN_POINT ( 'NONE',  ( -4.528983652092210654, 43.00000000000000000, 5.879373928346826261 ) ) ;
#2304 = DIRECTION ( 'NONE',  ( 1.000000000000000000, 0.000000000000000000, 0.000000000000000000 ) ) ;
#2305 = DIRECTION ( 'NONE',  ( 0.000000000000000000, -1.000000000000000000, 0.000000000000000000 ) ) ;
#2306 = EDGE_CURVE ( 'NONE', #1870, #1550, #2981, .T. ) ;
#2307 = VERTEX_POINT ( 'NONE', #292 ) ;
#2308 = VECTOR ( 'NONE', #1549, 1000.000000000000000 ) ;
#2309 = DIRECTION ( 'NONE',  ( 0.000000000000000000, 0.000000000000000000, 1.000000000000000000 ) ) ;
#2310 = DIRECTION ( 'NONE',  ( -0.000000000000000000, -1.000000000000000000, 0.000000000000000000 ) ) ;
#2311 = CIRCLE ( 'NONE', #4081, 1.000000000000000000 ) ;
#2312 = CARTESIAN_POINT ( 'NONE',  ( -19.41638709359449422, 22.87032942663237378, 5.821272343678753458 ) ) ;
#2313 = CARTESIAN_POINT ( 'NONE',  ( 3.872084230669218918, 34.73127030857578745, 10.00969786038576714 ) ) ;
#2314 = AXIS2_PLACEMENT_3D ( 'NONE', #2160, #1425, #5 ) ;
#2315 = DIRECTION ( 'NONE',  ( 0.000000000000000000, 0.000000000000000000, 1.000000000000000000 ) ) ;
#2316 = EDGE_LOOP ( 'NONE', ( #2732, #3638, #3020, #4066, #3679, #2871, #3812, #3526, #2804 ) ) ;
#2317 = ORIENTED_EDGE ( 'NONE', *, *, #724, .F. ) ;
#2318 = ORIENTED_EDGE ( 'NONE', *, *, #2236, .T. ) ;
#2319 = ORIENTED_EDGE ( 'NONE', *, *, #2646, .F. ) ;
#2320 = FACE_OUTER_BOUND ( 'NONE', #372, .T. ) ;
#2321 = DIRECTION ( 'NONE',  ( 0.000000000000000000, 0.000000000000000000, 1.000000000000000000 ) ) ;
#2322 = CARTESIAN_POINT ( 'NONE',  ( -4.528983652092209766, 37.00000000000000000, 5.879373928346827149 ) ) ;
#2323 = DIRECTION ( 'NONE',  ( 0.000000000000000000, 0.000000000000000000, 1.000000000000000000 ) ) ;
#2324 = DIRECTION ( 'NONE',  ( 1.000000000000000000, 0.000000000000000000, -0.000000000000000000 ) ) ;
#2325 = VECTOR ( 'NONE', #2467, 1000.000000000000000 ) ;
#2326 = ORIENTED_EDGE ( 'NONE', *, *, #3794, .F. ) ;
#2327 = AXIS2_PLACEMENT_3D ( 'NONE', #3982, #723, #4124 ) ;
#2328 = CARTESIAN_POINT ( 'NONE',  ( -1.773386257881301553, 29.94852044693267246, 12.59496732558994125 ) ) ;
#2329 = EDGE_CURVE ( 'NONE', #4361, #2996, #3864, .T. ) ;
#2330=STYLED_ITEM('',(#4729),#3033);
#2331 = FACE_OUTER_BOUND ( 'NONE', #1541, .T. ) ;
#2332 = AXIS2_PLACEMENT_3D ( 'NONE', #120, #2651, #4116 ) ;
#2333 = DIRECTION ( 'NONE',  ( -1.000000000000000000, 0.000000000000000000, 0.000000000000000000 ) ) ;
#2334 = FACE_OUTER_BOUND ( 'NONE', #105, .T. ) ;
#2335 = CARTESIAN_POINT ( 'NONE',  ( -19.58805710660148236, 17.18149551509898743, 20.00001200000000523 ) ) ;
#2336 = ORIENTED_EDGE ( 'NONE', *, *, #1647, .F. ) ;
#2337 = ORIENTED_EDGE ( 'NONE', *, *, #579, .T. ) ;
#2338 = VERTEX_POINT ( 'NONE', #4293 ) ;
#2339 = VERTEX_POINT ( 'NONE', #244 ) ;
#2340 = FACE_OUTER_BOUND ( 'NONE', #747, .T. ) ;
#2341 = DIRECTION ( 'NONE',  ( 0.000000000000000000, 0.000000000000000000, -1.000000000000000000 ) ) ;
#2342 =( NAMED_UNIT ( * ) PLANE_ANGLE_UNIT ( ) SI_UNIT ( $, .RADIAN. ) );
#2343 = SURFACE_STYLE_USAGE ( .BOTH. , #155 ) ;
#2344 = DIRECTION ( 'NONE',  ( 0.000000000000000000, 1.000000000000000000, 0.000000000000000000 ) ) ;
#2345 = CIRCLE ( 'NONE', #1907, 26.00000000000000711 ) ;
#2346 = CARTESIAN_POINT ( 'NONE',  ( -27.10000000000000497, 0.6000000000000000888, 19.59999999999999787 ) ) ;
#2347 = FACE_OUTER_BOUND ( 'NONE', #1929, .T. ) ;
#2348 = DIRECTION ( 'NONE',  ( 8.881784197001260212E-16, 0.000000000000000000, 1.000000000000000000 ) ) ;
#2349 = ORIENTED_EDGE ( 'NONE', *, *, #2214, .T. ) ;
#2350 = ADVANCED_FACE ( 'NONE', ( #1693 ), #3145, .F. ) ;
#2351 = CARTESIAN_POINT ( 'NONE',  ( -3.595408253811773758, 29.78394301743083261, 10.77252090037689136 ) ) ;
#2352 = EDGE_CURVE ( 'NONE', #4496, #4595, #635, .T. ) ;
#2353 = LINE ( 'NONE', #1629, #2390 ) ;
#2354 = CIRCLE ( 'NONE', #4045, 4.000000000000000000 ) ;
#2355 = EDGE_CURVE ( 'NONE', #1930, #525, #2763, .T. ) ;
#2356 = ADVANCED_FACE ( 'NONE', ( #2418 ), #3661, .T. ) ;
#2357 = DIRECTION ( 'NONE',  ( 0.000000000000000000, 0.000000000000000000, -1.000000000000000000 ) ) ;
#2358 = CARTESIAN_POINT ( 'NONE',  ( 0.000000000000000000, 0.000000000000000000, 18.19999999999999929 ) ) ;
#2359 = AXIS2_PLACEMENT_3D ( 'NONE', #1364, #2466, #1385 ) ;
#2360 = CARTESIAN_POINT ( 'NONE',  ( 0.000000000000000000, 3.469446951953614189E-15, 8.999999999999991118 ) ) ;
#2361 = CARTESIAN_POINT ( 'NONE',  ( -0.5000000000000000000, 0.8660254037844387076, 19.50000000000000000 ) ) ;
#2362 = ORIENTED_EDGE ( 'NONE', *, *, #4531, .F. ) ;
#2363 = ORIENTED_EDGE ( 'NONE', *, *, #4242, .F. ) ;
#2364 = ORIENTED_EDGE ( 'NONE', *, *, #3418, .T. ) ;
#2365 = ORIENTED_EDGE ( 'NONE', *, *, #3432, .T. ) ;
#2366 = DIRECTION ( 'NONE',  ( 0.000000000000000000, 0.000000000000000000, 1.000000000000000000 ) ) ;
#2367 = SURFACE_STYLE_FILL_AREA ( #3497 ) ;
#2368 =( NAMED_UNIT ( * ) PLANE_ANGLE_UNIT ( ) SI_UNIT ( $, .RADIAN. ) );
#2369 = DIRECTION ( 'NONE',  ( 0.000000000000000000, 0.000000000000000000, -1.000000000000000000 ) ) ;
#2370 = DIRECTION ( 'NONE',  ( 1.000000000000000000, 0.000000000000000000, 0.000000000000000000 ) ) ;
#2371 = DIRECTION ( 'NONE',  ( 0.000000000000000000, 0.000000000000000000, 1.000000000000000000 ) ) ;
#2372 = CARTESIAN_POINT ( 'NONE',  ( -0.7500000000000001110, 0.000000000000000000, 17.69999999999999929 ) ) ;
#2373 = ORIENTED_EDGE ( 'NONE', *, *, #2918, .F. ) ;
#2374 = CIRCLE ( 'NONE', #3453, 4.000000000000000000 ) ;
#2375 = AXIS2_PLACEMENT_3D ( 'NONE', #3819, #1254, #1672 ) ;
#2376 = CARTESIAN_POINT ( 'NONE',  ( 20.83769629064231665, 21.58369355588040861, 12.97362800538644301 ) ) ;
#2377 = EDGE_CURVE ( 'NONE', #741, #305, #1149, .T. ) ;
#2378 = LINE ( 'NONE', #232, #3536 ) ;
#2379 = CIRCLE ( 'NONE', #1107, 8.000000000000000000 ) ;
#2380 = CARTESIAN_POINT ( 'NONE',  ( -21.39687781493365293, 21.02954719696279895, 4.999903794384585431 ) ) ;
#2381 = DIRECTION ( 'NONE',  ( 0.000000000000000000, 0.000000000000000000, 1.000000000000000000 ) ) ;
#2382 = DIRECTION ( 'NONE',  ( 0.000000000000000000, 0.000000000000000000, 1.000000000000000000 ) ) ;
#2383 = EDGE_LOOP ( 'NONE', ( #1849, #4478 ) ) ;
#2384 = STYLED_ITEM ( 'NONE', ( #1641 ), #1996 ) ;
#2385 = VERTEX_POINT ( 'NONE', #3640 ) ;
#2386 = EDGE_LOOP ( 'NONE', ( #4145, #95 ) ) ;
#2387 = DIRECTION ( 'NONE',  ( 0.000000000000000000, 0.000000000000000000, 1.000000000000000000 ) ) ;
#2388 = ADVANCED_FACE ( 'NONE', ( #1785 ), #4335, .T. ) ;
#2389 = SURFACE_SIDE_STYLE ('',( #2367 ) ) ;
#2390 = VECTOR ( 'NONE', #2310, 1000.000000000000000 ) ;
#2391 =( NAMED_UNIT ( * ) SI_UNIT ( $, .STERADIAN. ) SOLID_ANGLE_UNIT ( ) );
#2392 = EDGE_CURVE ( 'NONE', #4090, #614, #379, .T. ) ;
#2393 = CYLINDRICAL_SURFACE ( 'NONE', #2535, 1.000000000000000000 ) ;
#2394 = CARTESIAN_POINT ( 'NONE',  ( 0.000000000000000000, 0.000000000000000000, 19.00000000000000000 ) ) ;
#2395 = EDGE_CURVE ( 'NONE', #1928, #2542, #3284, .T. ) ;
#2396 = DIRECTION ( 'NONE',  ( -0.000000000000000000, -0.000000000000000000, -1.000000000000000000 ) ) ;
#2397 = SHAPE_REPRESENTATION ( 'MAS-171', ( #1416, #3853, #1866, #969, #662, #3927, #3088, #2545, #3615 ), #3691 ) ;
#2398 = FACE_OUTER_BOUND ( 'NONE', #1615, .T. ) ;
#2399 = CARTESIAN_POINT ( 'NONE',  ( 0.5000000000000000000, -2.999999999999999556, 19.50000000000000000 ) ) ;
#2400 = EDGE_LOOP ( 'NONE', ( #3401, #2896, #2815, #3828 ) ) ;
#2401 = CARTESIAN_POINT ( 'NONE',  ( 1.500000000000000222, 0.000000000000000000, 17.69999999999999929 ) ) ;
#2402 = CARTESIAN_POINT ( 'NONE',  ( 3.889087296525981063, 49.00000000000000000, 12.88908729652603746 ) ) ;
#2403 = CARTESIAN_POINT ( 'NONE',  ( 25.99307600111999150, 0.5999999999999998668, 19.00000000000000000 ) ) ;
#2404 = CONICAL_SURFACE ( 'NONE', #1887, 4.000000000000000000, 0.7853981633974447263 ) ;
#2405 = DIRECTION ( 'NONE',  ( 1.000000000000000000, 0.000000000000000000, 0.000000000000000000 ) ) ;
#2406 = VECTOR ( 'NONE', #1360, 1000.000000000000000 ) ;
#2407 = LINE ( 'NONE', #4568, #1893 ) ;
#2408 = CARTESIAN_POINT ( 'NONE',  ( 0.5000000000000000000, -2.999999999999999556, 19.50000000000000000 ) ) ;
#2409 = EDGE_LOOP ( 'NONE', ( #1978, #3352 ) ) ;
#2410 = ORIENTED_EDGE ( 'NONE', *, *, #50, .T. ) ;
#2411 = DIRECTION ( 'NONE',  ( 0.7071067811865487940, 0.7071067811865463515, 0.000000000000000000 ) ) ;
#2412 = LINE ( 'NONE', #1400, #1232 ) ;
#2413 = EDGE_CURVE ( 'NONE', #1643, #3785, #4471, .T. ) ;
#2414 = SHAPE_REPRESENTATION_RELATIONSHIP ( 'NONE' , 'NONE' ,  #404, #4678 ) ;
#2415 = LINE ( 'NONE', #2461, #413 ) ;
#2416 = PRODUCT_DEFINITION_CONTEXT ( 'detailed design', #35, 'design' ) ;
#2417 = DIRECTION ( 'NONE',  ( 0.000000000000000000, -0.000000000000000000, 1.000000000000000000 ) ) ;
#2418 = FACE_OUTER_BOUND ( 'NONE', #2917, .T. ) ;
#2419 = DIRECTION ( 'NONE',  ( 0.000000000000000000, 1.000000000000000000, 0.000000000000000000 ) ) ;
#2420 = ADVANCED_FACE ( 'NONE', ( #4703 ), #3710, .T. ) ;
#2421 = CARTESIAN_POINT ( 'NONE',  ( 3.999815009702282875, 29.73216238221898067, 9.267216418983164061 ) ) ;
#2422 = EDGE_CURVE ( 'NONE', #3310, #3324, #2145, .T. ) ;
#2423 = EDGE_LOOP ( 'NONE', ( #3539, #3282, #304, #1635 ) ) ;
#2424 = AXIS2_PLACEMENT_3D ( 'NONE', #352, #3879, #4623 ) ;
#2425 = CARTESIAN_POINT ( 'NONE',  ( -3.015186248472646824, 29.84868090056883716, 11.64163568064553544 ) ) ;
#2426 = CARTESIAN_POINT ( 'NONE',  ( -3.403349963601427053, -25.83240171513484640, 20.00001199999999812 ) ) ;
#2427 = CARTESIAN_POINT ( 'NONE',  ( 3.469446951953614189E-15, 39.99999999999999289, 8.999999999999992895 ) ) ;
#2428 = FACE_OUTER_BOUND ( 'NONE', #3876, .T. ) ;
#2429 = EDGE_CURVE ( 'NONE', #3445, #4670, #3484, .T. ) ;
#2430 = AXIS2_PLACEMENT_3D ( 'NONE', #1143, #373, #830 ) ;
#2431 = CYLINDRICAL_SURFACE ( 'NONE', #2169, 26.00000000000000355 ) ;
#2432 = CIRCLE ( 'NONE', #318, 27.99999999999999645 ) ;
#2433 = ORIENTED_EDGE ( 'NONE', *, *, #3215, .F. ) ;
#2434 = EDGE_LOOP ( 'NONE', ( #3140, #4533 ) ) ;
#2435 = FACE_OUTER_BOUND ( 'NONE', #4002, .T. ) ;
#2436 = VECTOR ( 'NONE', #4530, 1000.000000000000000 ) ;
#2437 = EDGE_CURVE ( 'NONE', #803, #4308, #2228, .T. ) ;
#2438 = PLANE ( 'NONE',  #380 ) ;
#2439 = CARTESIAN_POINT ( 'NONE',  ( -8.377607117416806304, 24.67207871933483787, 20.00001200000000168 ) ) ;
#2440 = DIRECTION ( 'NONE',  ( 0.000000000000000000, 0.000000000000000000, 1.000000000000000000 ) ) ;
#2441 = DIRECTION ( 'NONE',  ( 0.000000000000000000, 0.000000000000000000, 1.000000000000000000 ) ) ;
#2442 = CARTESIAN_POINT ( 'NONE',  ( 3.014458645203628606, 29.84873923156943576, 6.357858316023347278 ) ) ;
#2443 = ORIENTED_EDGE ( 'NONE', *, *, #4560, .T. ) ;
#2444 = SURFACE_SIDE_STYLE ('',( #1368 ) ) ;
#2445 = PRODUCT_RELATED_PRODUCT_CATEGORY ( 'part', '', ( #3390 ) ) ;
#2446 = APPLICATION_CONTEXT ( 'automotive_design' ) ;
#2447 = PLANE ( 'NONE',  #2684 ) ;
#2448 = DIRECTION ( 'NONE',  ( 1.000000000000000000, 0.000000000000000000, 0.000000000000000000 ) ) ;
#2449 = EDGE_CURVE ( 'NONE', #4376, #1315, #3552, .T. ) ;
#2450 = VECTOR ( 'NONE', #18, 1000.000000000000000 ) ;
#2451 = CARTESIAN_POINT ( 'NONE',  ( 3.403349963601436823, -25.83240171513484995, 20.00001200000000878 ) ) ;
#2452 = AXIS2_PLACEMENT_3D ( 'NONE', #246, #894, #1986 ) ;
#2453 = LINE ( 'NONE', #712, #3582 ) ;
#2454 = CARTESIAN_POINT ( 'NONE',  ( 8.999999999999984013, 32.99999999999999289, 0.000000000000000000 ) ) ;
#2455 = PLANE ( 'NONE',  #3311 ) ;
#2456 = CIRCLE ( 'NONE', #4607, 4.000000000000000000 ) ;
#2457 = ORIENTED_EDGE ( 'NONE', *, *, #45, .F. ) ;
#2458 = ORIENTED_EDGE ( 'NONE', *, *, #199, .F. ) ;
#2459 = DIRECTION ( 'NONE',  ( -0.000000000000000000, -1.000000000000000000, -0.000000000000000000 ) ) ;
#2460 = CARTESIAN_POINT ( 'NONE',  ( 0.000000000000000000, 0.000000000000000000, 20.00001200000000168 ) ) ;
#2461 = CARTESIAN_POINT ( 'NONE',  ( 26.49999999999999645, -0.5000000000000000000, 19.00000000000000000 ) ) ;
#2462 = CARTESIAN_POINT ( 'NONE',  ( 3.469446951953614189E-15, 43.00000000000000000, 8.999999999999992895 ) ) ;
#2463 = ORIENTED_EDGE ( 'NONE', *, *, #2449, .F. ) ;
#2464 = CARTESIAN_POINT ( 'NONE',  ( 0.000000000000000000, 0.000000000000000000, 18.19999999999999929 ) ) ;
#2465 = CIRCLE ( 'NONE', #136, 26.00000000000000711 ) ;
#2466 = DIRECTION ( 'NONE',  ( 0.000000000000000000, 1.000000000000000000, 0.000000000000000000 ) ) ;
#2467 = DIRECTION ( 'NONE',  ( -0.000000000000000000, 1.000000000000000000, -0.000000000000000000 ) ) ;
#2468 = DIRECTION ( 'NONE',  ( -1.621111868633889227E-15, -1.000000000000000000, 0.000000000000000000 ) ) ;
#2469 =( GEOMETRIC_REPRESENTATION_CONTEXT ( 3 ) GLOBAL_UNCERTAINTY_ASSIGNED_CONTEXT ( ( #153 ) ) GLOBAL_UNIT_ASSIGNED_CONTEXT ( ( #374, #1164, #397 ) ) REPRESENTATION_CONTEXT ( 'NONE', 'WORKASPACE' ) );
#2470 = AXIS2_PLACEMENT_3D ( 'NONE', #2462, #2117, #26 ) ;
#2471 =( NAMED_UNIT ( * ) SI_UNIT ( $, .STERADIAN. ) SOLID_ANGLE_UNIT ( ) );
#2472 = LINE ( 'NONE', #2080, #3905 ) ;
#2473 = APPLICATION_PROTOCOL_DEFINITION ( 'draft international standard', 'automotive_design', 1998, #4178 ) ;
#2474 = CARTESIAN_POINT ( 'NONE',  ( -15.85973458909327150, -20.67279826512042362, 20.00001200000000168 ) ) ;
#2475 = EDGE_CURVE ( 'NONE', #4670, #3343, #3026, .T. ) ;
#2476 = DIRECTION ( 'NONE',  ( 0.000000000000000000, 1.000000000000000000, 0.000000000000000000 ) ) ;
#2477 = CYLINDRICAL_SURFACE ( 'NONE', #1776, 4.000000000000000000 ) ;
#2478 = AXIS2_PLACEMENT_3D ( 'NONE', #314, #3936, #270 ) ;
#2479 = CARTESIAN_POINT ( 'NONE',  ( 0.000000000000000000, 10.00000000000000000, 15.00000000000000178 ) ) ;
#2480 = ADVANCED_FACE ( 'NONE', ( #9, #2906 ), #4316, .F. ) ;
#2481 = ORIENTED_EDGE ( 'NONE', *, *, #3804, .F. ) ;
#2482 = VERTEX_POINT ( 'NONE', #2516 ) ;
#2483 = VECTOR ( 'NONE', #2048, 1000.000000000000000 ) ;
#2484 = CARTESIAN_POINT ( 'NONE',  ( 3.469446951953614189E-15, 25.00000000000000000, 8.999999999999992895 ) ) ;
#2485 = SURFACE_STYLE_USAGE ( .BOTH. , #4264 ) ;
#2486 = DIRECTION ( 'NONE',  ( -0.000000000000000000, -1.000000000000000000, -0.000000000000000000 ) ) ;
#2487 = CIRCLE ( 'NONE', #4106, 4.000000000000000000 ) ;
#2488 = ORIENTED_EDGE ( 'NONE', *, *, #4059, .T. ) ;
#2489 = DIRECTION ( 'NONE',  ( 0.000000000000000000, 0.000000000000000000, 1.000000000000000000 ) ) ;
#2490 = CARTESIAN_POINT ( 'NONE',  ( -17.67766952966371719, 17.67766952966366389, 8.999999999999992895 ) ) ;
#2491 = CIRCLE ( 'NONE', #3364, 26.00000000000000711 ) ;
#2492 = CIRCLE ( 'NONE', #3715, 1.749999999999999778 ) ;
#2493 = DIRECTION ( 'NONE',  ( 1.000000000000000000, -1.621111868633889227E-15, 0.000000000000000000 ) ) ;
#2494 = DIRECTION ( 'NONE',  ( -0.000000000000000000, -0.000000000000000000, 1.000000000000000000 ) ) ;
#2495 = EDGE_CURVE ( 'NONE', #3886, #2734, #4380, .T. ) ;
#2496 = CYLINDRICAL_SURFACE ( 'NONE', #3179, 5.000000000000001776 ) ;
#2497 = CARTESIAN_POINT ( 'NONE',  ( 23.85222316637486983, 18.19536891688241198, 9.264542937126584832 ) ) ;
#2498 = APPLICATION_PROTOCOL_DEFINITION ( 'draft international standard', 'automotive_design', 1998, #920 ) ;
#2499 = EDGE_CURVE ( 'NONE', #4272, #1192, #2204, .T. ) ;
#2500 = ADVANCED_BREP_SHAPE_REPRESENTATION ( '', ( #2883, #2928 ), #656 ) ;
#2501 = VECTOR ( 'NONE', #2759, 1000.000000000000000 ) ;
#2502 = ADVANCED_FACE ( 'NONE', ( #1055 ), #1407, .T. ) ;
#2503 = LINE ( 'NONE', #1704, #1455 ) ;
#2504 = CARTESIAN_POINT ( 'NONE',  ( 8.999999999999984013, 32.99999999999999289, -1.749999999999999778 ) ) ;
#2505 = CARTESIAN_POINT ( 'NONE',  ( -0.7500000000000000000, -2.999999999999999556, 18.19999999999999929 ) ) ;
#2506 = ORIENTED_EDGE ( 'NONE', *, *, #727, .F. ) ;
#2507 = ORIENTED_EDGE ( 'NONE', *, *, #459, .F. ) ;
#2508 = DIRECTION ( 'NONE',  ( 0.000000000000000000, 0.000000000000000000, -1.000000000000000000 ) ) ;
#2509=STYLED_ITEM('',(#4736),#1412);
#2510 = EDGE_CURVE ( 'NONE', #3253, #2903, #4404, .T. ) ;
#2511 = DIRECTION ( 'NONE',  ( 0.000000000000000000, -0.000000000000000000, 1.000000000000000000 ) ) ;
#2512 = ORIENTED_EDGE ( 'NONE', *, *, #2191, .F. ) ;
#2513 = CARTESIAN_POINT ( 'NONE',  ( 13.02991752792603108, 22.56362157461194329, 20.00001200000000168 ) ) ;
#2514 = AXIS2_PLACEMENT_3D ( 'NONE', #4109, #865, #1913 ) ;
#2515 = APPLICATION_CONTEXT ( 'automotive_design' ) ;
#2516 = CARTESIAN_POINT ( 'NONE',  ( -0.5000000000000001110, 10.00000000000000000, 13.00000000000000178 ) ) ;
#2517 = CYLINDRICAL_SURFACE ( 'NONE', #3800, 1.000000000000000000 ) ;
#2518 = CARTESIAN_POINT ( 'NONE',  ( 3.182992266941310433, 29.83102156157410434, 6.563430084856013202 ) ) ;
#2519 = CARTESIAN_POINT ( 'NONE',  ( 0.7500000000000000000, 0.000000000000000000, 17.69999999999999929 ) ) ;
#2520 = CARTESIAN_POINT ( 'NONE',  ( 23.72542776831235400, 18.36067068532939572, 10.29518969959635477 ) ) ;
#2521 = ITEM_DEFINED_TRANSFORMATION ( 'NONE', 'NONE', #969,  #2928 ) ;
#2522 = DIRECTION ( 'NONE',  ( 0.000000000000000000, 0.000000000000000000, 1.000000000000000000 ) ) ;
#2523 = DIRECTION ( 'NONE',  ( 0.000000000000000000, 1.000000000000000000, 0.000000000000000000 ) ) ;
#2524 = CARTESIAN_POINT ( 'NONE',  ( -4.528983652092254175, 43.00000000000000000, 12.12062607165309558 ) ) ;
#2525 = ORIENTED_EDGE ( 'NONE', *, *, #2437, .T. ) ;
#2526 = EDGE_LOOP ( 'NONE', ( #2018, #117, #69, #3908 ) ) ;
#2527 = CIRCLE ( 'NONE', #2225, 5.500000000000000000 ) ;
#2528 = CARTESIAN_POINT ( 'NONE',  ( 0.5000000000000000000, 6.000000000000000000, 19.50000000000000000 ) ) ;
#2529 =( NAMED_UNIT ( * ) SI_UNIT ( $, .STERADIAN. ) SOLID_ANGLE_UNIT ( ) );
#2530 = AXIS2_PLACEMENT_3D ( 'NONE', #2035, #2668, #2053 ) ;
#2531 = FACE_OUTER_BOUND ( 'NONE', #3786, .T. ) ;
#2532 = EDGE_LOOP ( 'NONE', ( #2656, #4200 ) ) ;
#2533 = ORIENTED_EDGE ( 'NONE', *, *, #2740, .T. ) ;
#2534 = ORIENTED_EDGE ( 'NONE', *, *, #542, .T. ) ;
#2535 = AXIS2_PLACEMENT_3D ( 'NONE', #3861, #605, #133 ) ;
#2536 = CARTESIAN_POINT ( 'NONE',  ( 26.49999999999999645, -0.5000000000000000000, 19.00000000000000000 ) ) ;
#2537 = EDGE_CURVE ( 'NONE', #3687, #4371, #3944, .T. ) ;
#2538 = EDGE_CURVE ( 'NONE', #3361, #1466, #1170, .T. ) ;
#2539 = CARTESIAN_POINT ( 'NONE',  ( 3.959305671612554781E-15, 33.00000000000000000, 12.99999999999999289 ) ) ;
#2540 = EDGE_CURVE ( 'NONE', #2196, #614, #3249, .T. ) ;
#2541 = LINE ( 'NONE', #2954, #2618 ) ;
#2542 = VERTEX_POINT ( 'NONE', #1271 ) ;
#2543 =( GEOMETRIC_REPRESENTATION_CONTEXT ( 3 ) GLOBAL_UNCERTAINTY_ASSIGNED_CONTEXT ( ( #3760 ) ) GLOBAL_UNIT_ASSIGNED_CONTEXT ( ( #4398, #1900, #2555 ) ) REPRESENTATION_CONTEXT ( 'NONE', 'WORKASPACE' ) );
#2544 = CARTESIAN_POINT ( 'NONE',  ( -5.409090909090905619, 33.00000000000000000, 8.999999999999992895 ) ) ;
#2545 = AXIS2_PLACEMENT_3D ( 'NONE', #3017, #904, #4277 ) ;
#2546 = CIRCLE ( 'NONE', #3168, 26.00000000000000355 ) ;
#2547 = FACE_OUTER_BOUND ( 'NONE', #2409, .T. ) ;
#2548 = APPLICATION_PROTOCOL_DEFINITION ( 'draft international standard', 'automotive_design', 1998, #2515 ) ;
#2549 = CARTESIAN_POINT ( 'NONE',  ( 23.77384460521241394, 18.29773070266329782, 7.963596978677151661 ) ) ;
#2550 = DIRECTION ( 'NONE',  ( 0.000000000000000000, 0.000000000000000000, 1.000000000000000000 ) ) ;
#2551 = FACE_OUTER_BOUND ( 'NONE', #3658, .T. ) ;
#2552 = VERTEX_POINT ( 'NONE', #152 ) ;
#2553 = VERTEX_POINT ( 'NONE', #4428 ) ;
#2554 = CARTESIAN_POINT ( 'NONE',  ( -3.672180636677252696, 31.77719734705737764, 7.412133430177195947 ) ) ;
#2555 =( NAMED_UNIT ( * ) SI_UNIT ( $, .STERADIAN. ) SOLID_ANGLE_UNIT ( ) );
#2556 = CARTESIAN_POINT ( 'NONE',  ( 0.000000000000000000, 10.00000000000000000, 15.00000000000000178 ) ) ;
#2557 = ORIENTED_EDGE ( 'NONE', *, *, #4589, .F. ) ;
#2558 = ORIENTED_EDGE ( 'NONE', *, *, #283, .T. ) ;
#2559 = ORIENTED_EDGE ( 'NONE', *, *, #2499, .F. ) ;
#2560 = CIRCLE ( 'NONE', #3628, 27.99999999999999645 ) ;
#2561 = DIRECTION ( 'NONE',  ( -0.000000000000000000, -0.000000000000000000, -1.000000000000000000 ) ) ;
#2562 = ADVANCED_FACE ( 'NONE', ( #530 ), #2612, .F. ) ;
#2563 = CARTESIAN_POINT ( 'NONE',  ( -21.58369355588047966, 20.83769629064224915, 12.97362800538644301 ) ) ;
#2564 = COLOUR_RGB ( '',0.8941176470588234615, 0.8941176470588234615, 0.8941176470588234615 ) ;
#2565 = FACE_BOUND ( 'NONE', #3933, .T. ) ;
#2566 = CARTESIAN_POINT ( 'NONE',  ( -1.701696020694465128, -26.00000000000001066, 20.00001200000000878 ) ) ;
#2567 = ORIENTED_EDGE ( 'NONE', *, *, #1066, .T. ) ;
#2568 = CIRCLE ( 'NONE', #4175, 0.5000000000000001110 ) ;
#2569 = EDGE_CURVE ( 'NONE', #3374, #4356, #2255, .T. ) ;
#2570 = ADVANCED_FACE ( 'NONE', ( #1880 ), #3711, .F. ) ;
#2571 = LINE ( 'NONE', #1201, #4143 ) ;
#2572 = PRODUCT_CONTEXT ( 'NONE', #422, 'mechanical' ) ;
#2573 = CIRCLE ( 'NONE', #3564, 1.000000000000000000 ) ;
#2574 = CARTESIAN_POINT ( 'NONE',  ( 27.09999999999999787, -0.5999999999999998668, 19.00000000000000000 ) ) ;
#2575 = DIRECTION ( 'NONE',  ( 1.000000000000000000, 0.000000000000000000, 0.000000000000000000 ) ) ;
#2576 = LINE ( 'NONE', #4040, #658 ) ;
#2577 = VERTEX_POINT ( 'NONE', #454 ) ;
#2578 = AXIS2_PLACEMENT_3D ( 'NONE', #3727, #49, #2948 ) ;
#2579 = ORIENTED_EDGE ( 'NONE', *, *, #3271, .T. ) ;
#2580 = CARTESIAN_POINT ( 'NONE',  ( 8.000000000000000000, 10.00000000000000000, 17.00000000000000000 ) ) ;
#2581 = EDGE_CURVE ( 'NONE', #3862, #1142, #1807, .T. ) ;
#2582 = CARTESIAN_POINT ( 'NONE',  ( 3.469446951953614189E-15, 25.00000000000000000, 8.999999999999992895 ) ) ;
#2583 = ORIENTED_EDGE ( 'NONE', *, *, #253, .T. ) ;
#2584 = EDGE_LOOP ( 'NONE', ( #3783, #3183 ) ) ;
#2585 = ORIENTED_EDGE ( 'NONE', *, *, #2095, .T. ) ;
#2586 = EDGE_CURVE ( 'NONE', #3868, #1490, #2644, .T. ) ;
#2587 = DIRECTION ( 'NONE',  ( -1.000000000000000000, 0.000000000000000000, 0.000000000000000000 ) ) ;
#2588 = CARTESIAN_POINT ( 'NONE',  ( -0.5000000000000001110, 10.00000000000000000, 13.00000000000000178 ) ) ;
#2589 = DIRECTION ( 'NONE',  ( -0.000000000000000000, -0.000000000000000000, 1.000000000000000000 ) ) ;
#2590 = CARTESIAN_POINT ( 'NONE',  ( -8.377607117416792093, -24.67207871933483787, 20.00001200000000168 ) ) ;
#2591 = CIRCLE ( 'NONE', #3801, 1.000000000000000000 ) ;
#2592 = CIRCLE ( 'NONE', #1084, 5.000000000000000888 ) ;
#2593 = ORIENTED_EDGE ( 'NONE', *, *, #1035, .T. ) ;
#2594 = CARTESIAN_POINT ( 'NONE',  ( 0.9958591954639605115, 43.00000000000000000, 3.590909090909087276 ) ) ;
#2595 = PRODUCT_DEFINITION_SHAPE ( 'NONE', 'NONE',  #4713 ) ;
#2596 = AXIS2_PLACEMENT_3D ( 'NONE', #3192, #584, #2034 ) ;
#2597 = DIRECTION ( 'NONE',  ( 0.000000000000000000, 0.000000000000000000, 1.000000000000000000 ) ) ;
#2598 = CONTEXT_DEPENDENT_SHAPE_REPRESENTATION ( #4082, #317 ) ;
#2599 = EDGE_CURVE ( 'NONE', #2044, #4376, #982, .T. ) ;
#2600 = DIRECTION ( 'NONE',  ( 1.224646799147350495E-16, 0.000000000000000000, -1.000000000000000000 ) ) ;
#2601 = CYLINDRICAL_SURFACE ( 'NONE', #2842, 0.9999999999999991118 ) ;
#2602 = CARTESIAN_POINT ( 'NONE',  ( 0.000000000000000000, 0.000000000000000000, 17.69999999999999929 ) ) ;
#2603 = ORIENTED_EDGE ( 'NONE', *, *, #1768, .T. ) ;
#2604 = ORIENTED_EDGE ( 'NONE', *, *, #4469, .F. ) ;
#2605 = EDGE_CURVE ( 'NONE', #377, #3402, #294, .T. ) ;
#2606 = DIRECTION ( 'NONE',  ( -0.000000000000000000, -1.000000000000000000, -0.000000000000000000 ) ) ;
#2607 = DIRECTION ( 'NONE',  ( 1.000000000000000000, 0.000000000000000000, 0.000000000000000000 ) ) ;
#2608 = VERTEX_POINT ( 'NONE', #2710 ) ;
#2609 = AXIS2_PLACEMENT_3D ( 'NONE', #1138, #3777, #2575 ) ;
#2610 = VERTEX_POINT ( 'NONE', #4147 ) ;
#2611 = ORIENTED_EDGE ( 'NONE', *, *, #611, .F. ) ;
#2612 = CYLINDRICAL_SURFACE ( 'NONE', #2723, 2.000000000000000888 ) ;
#2613 = DIRECTION ( 'NONE',  ( 0.000000000000000000, 1.000000000000000000, 0.000000000000000000 ) ) ;
#2614 = VECTOR ( 'NONE', #2149, 1000.000000000000000 ) ;
#2615 = CARTESIAN_POINT ( 'NONE',  ( 0.000000000000000000, 0.000000000000000000, 17.69999999999999929 ) ) ;
#2616 = DIRECTION ( 'NONE',  ( -0.000000000000000000, -1.000000000000000000, -0.000000000000000000 ) ) ;
#2617 = ORIENTED_EDGE ( 'NONE', *, *, #2057, .F. ) ;
#2618 = VECTOR ( 'NONE', #1104, 1000.000000000000000 ) ;
#2619 = CARTESIAN_POINT ( 'NONE',  ( -0.5000000000000000000, -2.999999999999999556, 19.50000000000000000 ) ) ;
#2620 = DIRECTION ( 'NONE',  ( -0.000000000000000000, 1.000000000000000000, 0.000000000000000000 ) ) ;
#2621 = STYLED_ITEM ( 'NONE', ( #3901 ), #4678 ) ;
#2622 = VECTOR ( 'NONE', #1420, 1000.000000000000000 ) ;
#2623 = CARTESIAN_POINT ( 'NONE',  ( 19.92346879083522637, 22.43020886076077502, 5.404597446377704451 ) ) ;
#2624 = FACE_OUTER_BOUND ( 'NONE', #4675, .T. ) ;
#2625 = CARTESIAN_POINT ( 'NONE',  ( -3.999956176514747774, 34.99991235301547476, 8.865408859660240282 ) ) ;
#2626 = CARTESIAN_POINT ( 'NONE',  ( 3.601840573626714281, 31.98585904651807965, 7.256529352857231885 ) ) ;
#2627 = EDGE_LOOP ( 'NONE', ( #2295, #1954, #8, #881 ) ) ;
#2628 = ORIENTED_EDGE ( 'NONE', *, *, #1556, .F. ) ;
#2629 = ADVANCED_FACE ( 'NONE', ( #2277 ), #2404, .T. ) ;
#2630 = CARTESIAN_POINT ( 'NONE',  ( -3.999885695961624243, 31.00022860814012660, 9.266511461428610374 ) ) ;
#2631 = CARTESIAN_POINT ( 'NONE',  ( 3.464101615137757051, 33.13239633626785974, 10.99999999999999645 ) ) ;
#2632 = EDGE_CURVE ( 'NONE', #4108, #213, #3327, .T. ) ;
#2633 = PLANE ( 'NONE',  #2738 ) ;
#2634 = ORIENTED_EDGE ( 'NONE', *, *, #696, .T. ) ;
#2635 = ORIENTED_EDGE ( 'NONE', *, *, #1520, .F. ) ;
#2636 = VERTEX_POINT ( 'NONE', #128 ) ;
#2637 = ORIENTED_EDGE ( 'NONE', *, *, #2537, .T. ) ;
#2638 = UNCERTAINTY_MEASURE_WITH_UNIT (LENGTH_MEASURE( 1.000000000000000082E-05 ), #3790, 'distance_accuracy_value', 'NONE');
#2639 = DIRECTION ( 'NONE',  ( 0.000000000000000000, 1.000000000000000000, 0.000000000000000000 ) ) ;
#2640 = DIRECTION ( 'NONE',  ( 1.000000000000000000, -8.560005772541128451E-15, 0.000000000000000000 ) ) ;
#2641 = DIRECTION ( 'NONE',  ( 0.000000000000000000, -1.000000000000000000, 0.000000000000000000 ) ) ;
#2642 = ORIENTED_EDGE ( 'NONE', *, *, #864, .F. ) ;
#2643 = LINE ( 'NONE', #510, #2825 ) ;
#2644 = CIRCLE ( 'NONE', #1791, 5.500000000000000000 ) ;
#2645 = DIRECTION ( 'NONE',  ( -0.000000000000000000, -0.000000000000000000, -1.000000000000000000 ) ) ;
#2646 = EDGE_CURVE ( 'NONE', #3706, #3472, #2560, .T. ) ;
#2647 = DIRECTION ( 'NONE',  ( 1.000000000000000000, 0.000000000000000000, 0.000000000000000000 ) ) ;
#2648 = FACE_OUTER_BOUND ( 'NONE', #351, .T. ) ;
#2649 = ORIENTED_EDGE ( 'NONE', *, *, #215, .T. ) ;
#2650 = CARTESIAN_POINT ( 'NONE',  ( -12.00000000000000000, 36.00000000000001421, 0.000000000000000000 ) ) ;
#2651 = DIRECTION ( 'NONE',  ( 0.000000000000000000, 1.000000000000000000, 0.000000000000000000 ) ) ;
#2652 = SURFACE_STYLE_USAGE ( .BOTH. , #660 ) ;
#2653 = DIRECTION ( 'NONE',  ( 0.000000000000000000, 1.000000000000000000, 0.000000000000000000 ) ) ;
#2654 = ORIENTED_EDGE ( 'NONE', *, *, #3709, .F. ) ;
#2655 = VECTOR ( 'NONE', #3346, 1000.000000000000000 ) ;
#2656 = ORIENTED_EDGE ( 'NONE', *, *, #3834, .F. ) ;
#2657 = VERTEX_POINT ( 'NONE', #4481 ) ;
#2658 = ORIENTED_EDGE ( 'NONE', *, *, #2755, .T. ) ;
#2659 = DIRECTION ( 'NONE',  ( -0.000000000000000000, -0.000000000000000000, -1.000000000000000000 ) ) ;
#2660 = ADVANCED_FACE ( 'NONE', ( #2320 ), #66, .T. ) ;
#2661 = DIRECTION ( 'NONE',  ( 0.000000000000000000, 0.000000000000000000, 1.000000000000000000 ) ) ;
#2662 = UNCERTAINTY_MEASURE_WITH_UNIT (LENGTH_MEASURE( 1.000000000000000082E-05 ), #2852, 'distance_accuracy_value', 'NONE');
#2663 =( NAMED_UNIT ( * ) PLANE_ANGLE_UNIT ( ) SI_UNIT ( $, .RADIAN. ) );
#2664 = CARTESIAN_POINT ( 'NONE',  ( 27.09999999999999787, -0.5999999999999998668, 19.59999999999999787 ) ) ;
#2665 = DIRECTION ( 'NONE',  ( 0.000000000000000000, 1.000000000000000000, 0.000000000000000000 ) ) ;
#2666 = CARTESIAN_POINT ( 'NONE',  ( 0.000000000000000000, 10.00000000000000000, 15.00000000000000178 ) ) ;
#2667=STYLED_ITEM('',(#4729),#1329);
#2668 = DIRECTION ( 'NONE',  ( -0.000000000000000000, -1.000000000000000000, -0.000000000000000000 ) ) ;
#2669 = VECTOR ( 'NONE', #4155, 1000.000000000000000 ) ;
#2670 = AXIS2_PLACEMENT_3D ( 'NONE', #3817, #1964, #1646 ) ;
#2671 = DIRECTION ( 'NONE',  ( 1.000000000000000000, 0.000000000000000000, 0.000000000000000000 ) ) ;
#2672 = DIRECTION ( 'NONE',  ( 0.000000000000000000, 0.000000000000000000, 1.000000000000000000 ) ) ;
#2673 = VECTOR ( 'NONE', #4518, 1000.000000000000000 ) ;
#2674 = FACE_OUTER_BOUND ( 'NONE', #3471, .T. ) ;
#2675 = CARTESIAN_POINT ( 'NONE',  ( 3.501495480098620217, 33.52633409191729186, 10.93402018205975779 ) ) ;
#2676 = DIRECTION ( 'NONE',  ( 0.000000000000000000, 0.000000000000000000, -1.000000000000000000 ) ) ;
#2677 = ORIENTED_EDGE ( 'NONE', *, *, #1725, .F. ) ;
#2678 = EDGE_LOOP ( 'NONE', ( #3844, #2951 ) ) ;
#2679 = VERTEX_POINT ( 'NONE', #910 ) ;
#2680 = VERTEX_POINT ( 'NONE', #3757 ) ;
#2681 = CARTESIAN_POINT ( 'NONE',  ( 3.469446951953614189E-15, 41.00000000000000000, 8.999999999999992895 ) ) ;
#2682 = CARTESIAN_POINT ( 'NONE',  ( -3.120626071653209710, 43.00000000000000000, 13.52898365209217246 ) ) ;
#2683 = FILL_AREA_STYLE ('',( #3985 ) ) ;
#2684 = AXIS2_PLACEMENT_3D ( 'NONE', #1793, #275, #730 ) ;
#2685 = LINE ( 'NONE', #4152, #4149 ) ;
#2686 = VERTEX_POINT ( 'NONE', #502 ) ;
#2687 = CIRCLE ( 'NONE', #4224, 0.9999999999999995559 ) ;
#2688 = ADVANCED_FACE ( 'NONE', ( #2340 ), #1959, .F. ) ;
#2689 = CARTESIAN_POINT ( 'NONE',  ( 0.5000000000000000000, 6.000000000000000000, 19.50000000000000000 ) ) ;
#2690 = EDGE_CURVE ( 'NONE', #2307, #715, #3814, .T. ) ;
#2691 = CARTESIAN_POINT ( 'NONE',  ( 0.000000000000000000, 0.000000000000000000, 15.00000000000000178 ) ) ;
#2692 = CARTESIAN_POINT ( 'NONE',  ( 0.7500000000000000000, -1.299038105676658450, 17.69999999999999929 ) ) ;
#2693 = ORIENTED_EDGE ( 'NONE', *, *, #2866, .T. ) ;
#2694 = AXIS2_PLACEMENT_3D ( 'NONE', #4505, #2301, #1248 ) ;
#2695 =( GEOMETRIC_REPRESENTATION_CONTEXT ( 3 ) GLOBAL_UNCERTAINTY_ASSIGNED_CONTEXT ( ( #1545 ) ) GLOBAL_UNIT_ASSIGNED_CONTEXT ( ( #651, #4625, #2808 ) ) REPRESENTATION_CONTEXT ( 'NONE', 'WORKASPACE' ) );
#2696 = CARTESIAN_POINT ( 'NONE',  ( 0.7500000000000001110, 0.000000000000000000, 15.00000000000000178 ) ) ;
#2697 = FACE_OUTER_BOUND ( 'NONE', #737, .T. ) ;
#2698 = STYLED_ITEM ( 'NONE', ( #4022 ), #4552 ) ;
#2699 = VECTOR ( 'NONE', #644, 1000.000000000000000 ) ;
#2700 = CARTESIAN_POINT ( 'NONE',  ( -19.92335677698585172, 22.43029000766435388, 5.404794703904383546 ) ) ;
#2701 = DIRECTION ( 'NONE',  ( 0.7071067811865462405, -0.7071067811865487940, 0.000000000000000000 ) ) ;
#2702 = PRODUCT_DEFINITION_SHAPE ( 'NONE', 'NONE',  #4711 ) ;
#2703 = CARTESIAN_POINT ( 'NONE',  ( 1.313779366493929901, 1.313779366493928347, 0.1938676166917873145 ) ) ;
#2704 = AXIS2_PLACEMENT_3D ( 'NONE', #4664, #2843, #4079 ) ;
#2705 = DIRECTION ( 'NONE',  ( 1.000000000000000000, 0.000000000000000000, 0.000000000000000000 ) ) ;
#2706 = ORIENTED_EDGE ( 'NONE', *, *, #3917, .T. ) ;
#2707 = VERTEX_POINT ( 'NONE', #959 ) ;
#2708 = ORIENTED_EDGE ( 'NONE', *, *, #1040, .F. ) ;
#2709 = ORIENTED_EDGE ( 'NONE', *, *, #2002, .T. ) ;
#2710 = CARTESIAN_POINT ( 'NONE',  ( 3.469446951953614189E-15, 37.00000000000000000, 4.999999999999992006 ) ) ;
#2711 = LINE ( 'NONE', #2682, #3810 ) ;
#2712 =( NAMED_UNIT ( * ) PLANE_ANGLE_UNIT ( ) SI_UNIT ( $, .RADIAN. ) );
#2713 = DIRECTION ( 'NONE',  ( 1.000000000000000000, 0.000000000000000000, 0.000000000000000000 ) ) ;
#2714 = DIRECTION ( 'NONE',  ( -0.000000000000000000, -0.000000000000000000, -1.000000000000000000 ) ) ;
#2715 = EDGE_CURVE ( 'NONE', #1468, #3612, #575, .T. ) ;
#2716 = CYLINDRICAL_SURFACE ( 'NONE', #322, 1.000000000000000000 ) ;
#2717 = DIRECTION ( 'NONE',  ( -0.000000000000000000, -1.000000000000000000, -0.000000000000000000 ) ) ;
#2718 = VECTOR ( 'NONE', #990, 1000.000000000000000 ) ;
#2719 = PLANE ( 'NONE',  #340 ) ;
#2720 = ORIENTED_EDGE ( 'NONE', *, *, #2862, .T. ) ;
#2721 = ADVANCED_FACE ( 'NONE', ( #2435 ), #3516, .T. ) ;
#2722 = ADVANCED_FACE ( 'NONE', ( #3096, #3474 ), #4240, .T. ) ;
#2723 = AXIS2_PLACEMENT_3D ( 'NONE', #813, #2973, #4500 ) ;
#2724 = CARTESIAN_POINT ( 'NONE',  ( 20.28006516365571699, 22.10831845702701060, 12.79440425686131988 ) ) ;
#2725 = DIRECTION ( 'NONE',  ( 0.000000000000000000, 1.000000000000000000, 0.000000000000000000 ) ) ;
#2726 = AXIS2_PLACEMENT_3D ( 'NONE', #545, #4168, #3135 ) ;
#2727 = DIRECTION ( 'NONE',  ( -0.000000000000000000, 1.000000000000000000, 0.000000000000000000 ) ) ;
#2728 = CARTESIAN_POINT ( 'NONE',  ( 4.081770351527290718E-15, 40.00000000000000000, 13.99999999999999467 ) ) ;
#2729 = DIRECTION ( 'NONE',  ( -0.1459754851659923747, -0.1459754851659928743, 0.9784591537009126316 ) ) ;
#2730 = FACE_OUTER_BOUND ( 'NONE', #3558, .T. ) ;
#2731 = VERTEX_POINT ( 'NONE', #4647 ) ;
#2732 = ORIENTED_EDGE ( 'NONE', *, *, #2352, .F. ) ;
#2733 = ORIENTED_EDGE ( 'NONE', *, *, #828, .F. ) ;
#2734 = VERTEX_POINT ( 'NONE', #3859 ) ;
#2735 = DIRECTION ( 'NONE',  ( -0.000000000000000000, -0.000000000000000000, -1.000000000000000000 ) ) ;
#2736 = CARTESIAN_POINT ( 'NONE',  ( 26.00000000000000711, 3.184081677783118980E-15, 20.00000000000000000 ) ) ;
#2737 = ORIENTED_EDGE ( 'NONE', *, *, #2057, .T. ) ;
#2738 = AXIS2_PLACEMENT_3D ( 'NONE', #1976, #1145, #3323 ) ;
#2739 = CYLINDRICAL_SURFACE ( 'NONE', #2596, 4.000000000000000000 ) ;
#2740 = EDGE_CURVE ( 'NONE', #4100, #3687, #1295, .T. ) ;
#2741 = DIRECTION ( 'NONE',  ( 0.000000000000000000, 0.000000000000000000, 1.000000000000000000 ) ) ;
#2742 = DIRECTION ( 'NONE',  ( -0.000000000000000000, -0.000000000000000000, -1.000000000000000000 ) ) ;
#2743 = EDGE_LOOP ( 'NONE', ( #2077, #1927, #2923, #3559, #4122, #3446, #3707, #992, #216 ) ) ;
#2744 = AXIS2_PLACEMENT_3D ( 'NONE', #3467, #3036, #3060 ) ;
#2745 = CARTESIAN_POINT ( 'NONE',  ( -3.974007292349814424, 29.73566758725665338, 9.525109153848150711 ) ) ;
#2746 = CARTESIAN_POINT ( 'NONE',  ( 3.469446951953614189E-15, 34.00000000000000000, 8.999999999999992895 ) ) ;
#2747 = CLOSED_SHELL ( 'NONE', ( #1099, #2420, #1211, #664, #3557, #2570, #3013, #1216, #1942, #3482 ) ) ;
#2748 = AXIS2_PLACEMENT_3D ( 'NONE', #2259, #2665, #4131 ) ;
#2749 = ADVANCED_FACE ( 'NONE', ( #3496 ), #2069, .T. ) ;
#2750 = ADVANCED_FACE ( 'NONE', ( #240 ), #4286, .F. ) ;
#2751 = CARTESIAN_POINT ( 'NONE',  ( -18.97646788767675119, 23.23634976112692740, 6.355262957884884045 ) ) ;
#2752 = DIRECTION ( 'NONE',  ( 0.000000000000000000, 0.000000000000000000, -1.000000000000000000 ) ) ;
#2753 = CARTESIAN_POINT ( 'NONE',  ( -22.56362157461194329, 13.02991752792602931, 20.00001200000000168 ) ) ;
#2754 = ORIENTED_EDGE ( 'NONE', *, *, #2495, .T. ) ;
#2755 = EDGE_CURVE ( 'NONE', #102, #1759, #552, .T. ) ;
#2756 = EDGE_LOOP ( 'NONE', ( #3809, #150, #1875, #2463 ) ) ;
#2757 = ORIENTED_EDGE ( 'NONE', *, *, #583, .F. ) ;
#2758 = DIRECTION ( 'NONE',  ( 0.000000000000000000, 1.000000000000000000, 0.000000000000000000 ) ) ;
#2759 = DIRECTION ( 'NONE',  ( -0.000000000000000000, -0.000000000000000000, -1.000000000000000000 ) ) ;
#2760 =( NAMED_UNIT ( * ) PLANE_ANGLE_UNIT ( ) SI_UNIT ( $, .RADIAN. ) );
#2761 = CARTESIAN_POINT ( 'NONE',  ( -0.7500000000000001110, 9.184850993605150903E-17, 15.00000000000000178 ) ) ;
#2762 = DIRECTION ( 'NONE',  ( 0.000000000000000000, 1.000000000000000000, 0.000000000000000000 ) ) ;
#2763 = LINE ( 'NONE', #653, #4506 ) ;
#2764 = CARTESIAN_POINT ( 'NONE',  ( -0.7500000000000001110, 0.000000000000000000, 17.69999999999999929 ) ) ;
#2765 = DIRECTION ( 'NONE',  ( 0.000000000000000000, 0.000000000000000000, 1.000000000000000000 ) ) ;
#2766 = EDGE_LOOP ( 'NONE', ( #2970, #3747, #434, #4042 ) ) ;
#2767 = B_SPLINE_CURVE_WITH_KNOTS ( 'NONE', 3,
 ( #3960, #2141, #3169, #1714, #4652, #1427, #2879, #1383, #2810, #2833, #1077, #2513, #3980, #629, #2073, #721, #3520, #2163, #242, #1005, #2439, #1683, #212, #4170, #1288, #2335, #1334, #2753, #1633, #187, #3827, #2065, #978, #569 ),
 .UNSPECIFIED., .F., .F.,
 ( 4, 2, 2, 2, 2, 2, 2, 2, 2, 2, 2, 2, 2, 2, 2, 2, 4 ),
 ( 0.000000000000000000, 0.03124999999999998612, 0.06249999999999995837, 0.09374999999999993061, 0.1249999999999999029, 0.1562499999999998890, 0.1874999999999998890, 0.2187499999999998890, 0.2499999999999998890, 0.2812499999999998890, 0.3124999999999998890, 0.3437499999999998335, 0.3749999999999998335, 0.4062499999999998335, 0.4374999999999998335, 0.4687499999999998890, 0.5000000000000000000 ),
 .UNSPECIFIED. ) ;
#2768 = AXIS2_PLACEMENT_3D ( 'NONE', #3366, #3695, #1944 ) ;
#2769 = VECTOR ( 'NONE', #3103, 1000.000000000000000 ) ;
#2770 = CARTESIAN_POINT ( 'NONE',  ( -0.2612076306139402004, 30.00000000000001066, 12.99999999999999467 ) ) ;
#2771 = DIRECTION ( 'NONE',  ( 0.000000000000000000, 0.000000000000000000, 1.000000000000000000 ) ) ;
#2772 = PRESENTATION_LAYER_ASSIGNMENT (  '', '', ( #3759 ) ) ;
#2773 = EDGE_CURVE ( 'NONE', #2542, #1466, #3107, .T. ) ;
#2774 = LINE ( 'NONE', #642, #1384 ) ;
#2775 = DIRECTION ( 'NONE',  ( 1.000000000000000000, 0.000000000000000000, 0.000000000000000000 ) ) ;
#2776 = FACE_OUTER_BOUND ( 'NONE', #1441, .T. ) ;
#2777 = ORIENTED_EDGE ( 'NONE', *, *, #1070, .T. ) ;
#2778 = VECTOR ( 'NONE', #1653, 1000.000000000000000 ) ;
#2779 = ORIENTED_EDGE ( 'NONE', *, *, #1586, .F. ) ;
#2780 = VERTEX_POINT ( 'NONE', #2023 ) ;
#2781 = EDGE_CURVE ( 'NONE', #3119, #3995, #2260, .T. ) ;
#2782 = DIRECTION ( 'NONE',  ( -0.000000000000000000, -0.000000000000000000, 1.000000000000000000 ) ) ;
#2783 = EDGE_CURVE ( 'NONE', #1759, #2850, #983, .T. ) ;
#2784 = DIRECTION ( 'NONE',  ( 0.000000000000000000, -1.000000000000000000, -0.000000000000000000 ) ) ;
#2785 = AXIS2_PLACEMENT_3D ( 'NONE', #2556, #1446, #1403 ) ;
#2786 =( NAMED_UNIT ( * ) PLANE_ANGLE_UNIT ( ) SI_UNIT ( $, .RADIAN. ) );
#2787 = PRODUCT ( 'minute hand', 'minute hand', '', ( #4688 ) ) ;
#2788 = LINE ( 'NONE', #1363, #3138 ) ;
#2789 = CARTESIAN_POINT ( 'NONE',  ( 3.469446951953614189E-15, 43.00000000000000000, 4.999999999999992006 ) ) ;
#2790 = DIRECTION ( 'NONE',  ( -0.000000000000000000, -1.000000000000000000, -0.000000000000000000 ) ) ;
#2791 = CARTESIAN_POINT ( 'NONE',  ( 2.646272448955801160, 29.88363158593299929, 5.989166937914467859 ) ) ;
#2792 = ORIENTED_EDGE ( 'NONE', *, *, #4212, .T. ) ;
#2793 = CARTESIAN_POINT ( 'NONE',  ( -5.499999999999996447, 49.00000000000000000, 8.999999999999992895 ) ) ;
#2794 = EDGE_CURVE ( 'NONE', #525, #2276, #2487, .T. ) ;
#2795 = APPLICATION_CONTEXT ( 'automotive_design' ) ;
#2796 = CARTESIAN_POINT ( 'NONE',  ( -3.871726839561290490, 29.74915783848840434, 10.03836643961818886 ) ) ;
#2797 = LINE ( 'NONE', #994, #1351 ) ;
#2798 = VECTOR ( 'NONE', #2805, 1000.000000000000000 ) ;
#2799 = DIRECTION ( 'NONE',  ( 0.000000000000000000, 0.000000000000000000, -1.000000000000000000 ) ) ;
#2800 = CIRCLE ( 'NONE', #4396, 0.9999999999999991118 ) ;
#2801 = CARTESIAN_POINT ( 'NONE',  ( 5.409090909090911836, 37.00000000000000000, 9.995859195463930646 ) ) ;
#2802 = DIRECTION ( 'NONE',  ( 0.000000000000000000, 0.000000000000000000, -1.000000000000000000 ) ) ;
#2803 = ORIENTED_EDGE ( 'NONE', *, *, #3093, .T. ) ;
#2804 = ORIENTED_EDGE ( 'NONE', *, *, #1768, .F. ) ;
#2805 = DIRECTION ( 'NONE',  ( -0.000000000000000000, -1.000000000000000000, -0.000000000000000000 ) ) ;
#2806 = PRESENTATION_STYLE_ASSIGNMENT (( #3229 ) ) ;
#2807 = FILL_AREA_STYLE_COLOUR ( '', #1037 ) ;
#2808 =( NAMED_UNIT ( * ) SI_UNIT ( $, .STERADIAN. ) SOLID_ANGLE_UNIT ( ) );
#2809 = PRODUCT_DEFINITION_CONTEXT ( 'detailed design', #3191, 'design' ) ;
#2810 = CARTESIAN_POINT ( 'NONE',  ( 19.58805710660146815, 17.18149551509899453, 20.00001200000000168 ) ) ;
#2811 = EDGE_CURVE ( 'NONE', #2036, #1146, #3833, .T. ) ;
#2812 = CARTESIAN_POINT ( 'NONE',  ( 26.49999999999999645, -0.5000000000000000000, 19.50000000000000000 ) ) ;
#2813 = DIRECTION ( 'NONE',  ( 0.000000000000000000, 0.000000000000000000, 1.000000000000000000 ) ) ;
#2814 = CARTESIAN_POINT ( 'NONE',  ( 0.2645425327012488337, 30.00000000000001066, 4.999999999999992006 ) ) ;
#2815 = ORIENTED_EDGE ( 'NONE', *, *, #54, .F. ) ;
#2816 = CIRCLE ( 'NONE', #768, 1.750000000000001554 ) ;
#2817 =( NAMED_UNIT ( * ) PLANE_ANGLE_UNIT ( ) SI_UNIT ( $, .RADIAN. ) );
#2818 = CARTESIAN_POINT ( 'NONE',  ( 13.75000000000001954, 44.99999999999999289, 0.000000000000000000 ) ) ;
#2819 = FILL_AREA_STYLE ('',( #522 ) ) ;
#2820 = PLANE ( 'NONE',  #2704 ) ;
#2821 = DIRECTION ( 'NONE',  ( 0.000000000000000000, -1.000000000000000000, 0.000000000000000000 ) ) ;
#2822 = CARTESIAN_POINT ( 'NONE',  ( -0.5000000000000000000, 0.8660254037844387076, 19.50000000000000000 ) ) ;
#2823 = PRODUCT_DEFINITION_SHAPE ( 'NONE', 'NONE',  #2956 ) ;
#2824 = CARTESIAN_POINT ( 'NONE',  ( -3.948082828799468480, 34.89455565685986471, 8.346052798592715760 ) ) ;
#2825 = VECTOR ( 'NONE', #2323, 1000.000000000000000 ) ;
#2826 = ORIENTED_EDGE ( 'NONE', *, *, #1177, .T. ) ;
#2827 = ORIENTED_EDGE ( 'NONE', *, *, #538, .F. ) ;
#2828 = DIRECTION ( 'NONE',  ( 1.000000000000000000, 0.000000000000000000, -0.000000000000000000 ) ) ;
#2829 = AXIS2_PLACEMENT_3D ( 'NONE', #3883, #2371, #4205 ) ;
#2830 = FACE_OUTER_BOUND ( 'NONE', #4160, .T. ) ;
#2831 = DIRECTION ( 'NONE',  ( -0.000000000000000000, -0.000000000000000000, 1.000000000000000000 ) ) ;
#2832 = EDGE_LOOP ( 'NONE', ( #4409, #1000, #7, #1544 ) ) ;
#2833 = CARTESIAN_POINT ( 'NONE',  ( 17.18149551509901940, 19.58805710660145039, 20.00001200000000168 ) ) ;
#2834 = DIRECTION ( 'NONE',  ( -0.000000000000000000, -0.000000000000000000, -1.000000000000000000 ) ) ;
#2835 = LINE ( 'NONE', #1786, #2718 ) ;
#2836 = CARTESIAN_POINT ( 'NONE',  ( 3.959305739469038251E-15, 30.00000000000000355, 12.99999999999999289 ) ) ;
#2837 = EDGE_CURVE ( 'NONE', #2135, #2482, #365, .T. ) ;
#2838 =( LENGTH_UNIT ( ) NAMED_UNIT ( * ) SI_UNIT ( .MILLI., .METRE. ) );
#2839 = EDGE_CURVE ( 'NONE', #3303, #3182, #3120, .T. ) ;
#2840 = PLANE ( 'NONE',  #264 ) ;
#2841 = DIRECTION ( 'NONE',  ( 0.000000000000000000, 0.000000000000000000, 1.000000000000000000 ) ) ;
#2842 = AXIS2_PLACEMENT_3D ( 'NONE', #439, #4440, #1581 ) ;
#2843 = DIRECTION ( 'NONE',  ( 0.000000000000000000, 0.000000000000000000, 1.000000000000000000 ) ) ;
#2844 = AXIS2_PLACEMENT_3D ( 'NONE', #139, #1578, #2597 ) ;
#2845 = FACE_OUTER_BOUND ( 'NONE', #1068, .T. ) ;
#2846 = FACE_OUTER_BOUND ( 'NONE', #2902, .T. ) ;
#2847 = DIRECTION ( 'NONE',  ( -1.927470528863123239E-16, 1.000000000000000000, 0.000000000000000000 ) ) ;
#2848 = AXIS2_PLACEMENT_3D ( 'NONE', #2231, #4458, #82 ) ;
#2849 = VERTEX_POINT ( 'NONE', #4574 ) ;
#2850 = VERTEX_POINT ( 'NONE', #625 ) ;
#2851 = DIRECTION ( 'NONE',  ( -0.000000000000000000, 1.000000000000000000, -0.000000000000000000 ) ) ;
#2852 =( LENGTH_UNIT ( ) NAMED_UNIT ( * ) SI_UNIT ( .MILLI., .METRE. ) );
#2853 = PLANE ( 'NONE',  #3692 ) ;
#2854 = VERTEX_POINT ( 'NONE', #648 ) ;
#2855 = CARTESIAN_POINT ( 'NONE',  ( -0.5000000000000000000, -0.8660254037844387076, 19.50000000000000000 ) ) ;
#2856 = MECHANICAL_DESIGN_GEOMETRIC_PRESENTATION_REPRESENTATION (  '', ( #3921 ), #3688 ) ;
#2857 = AXIS2_PLACEMENT_3D ( 'NONE', #2602, #42, #3317 ) ;
#2858 = DIRECTION ( 'NONE',  ( -1.000000000000000000, 0.000000000000000000, 0.000000000000000000 ) ) ;
#2859 = LINE ( 'NONE', #293, #2325 ) ;
#2860 = CARTESIAN_POINT ( 'NONE',  ( 3.974400453438903025, 29.73561427688381187, 8.478299341892736152 ) ) ;
#2861 = EDGE_CURVE ( 'NONE', #668, #3799, #1294, .T. ) ;
#2862 = EDGE_CURVE ( 'NONE', #102, #3297, #285, .T. ) ;
#2863 = CARTESIAN_POINT ( 'NONE',  ( 0.7500000000000001110, 20.00000000000000000, 17.69999999999999929 ) ) ;
#2864 = CARTESIAN_POINT ( 'NONE',  ( 30.00000000000000355, 3.673940397442059967E-15, 17.99999999999998579 ) ) ;
#2865 = ADVANCED_FACE ( 'NONE', ( #670 ), #3562, .F. ) ;
#2866 = EDGE_CURVE ( 'NONE', #2339, #4090, #4250, .T. ) ;
#2867 = FACE_OUTER_BOUND ( 'NONE', #4572, .T. ) ;
#2868 = DIRECTION ( 'NONE',  ( 1.000000000000000000, 0.000000000000000000, 0.000000000000000000 ) ) ;
#2869 = CIRCLE ( 'NONE', #4545, 0.5000000000000001110 ) ;
#2870 = CARTESIAN_POINT ( 'NONE',  ( -3.889087296526055226, 37.00000000000000000, 12.88908729652595753 ) ) ;
#2871 = ORIENTED_EDGE ( 'NONE', *, *, #4271, .F. ) ;
#2872 = ORIENTED_EDGE ( 'NONE', *, *, #4560, .F. ) ;
#2873 = VECTOR ( 'NONE', #4596, 1000.000000000000000 ) ;
#2874 = LINE ( 'NONE', #1049, #3277 ) ;
#2875 = PLANE ( 'NONE',  #3764 ) ;
#2876 = DIRECTION ( 'NONE',  ( 0.000000000000000000, 0.000000000000000000, -1.000000000000000000 ) ) ;
#2877 = COLOUR_RGB ( '',0.8941176470588234615, 0.8941176470588234615, 0.8941176470588234615 ) ;
#2878 = VERTEX_POINT ( 'NONE', #2863 ) ;
#2879 = CARTESIAN_POINT ( 'NONE',  ( 22.56362157461193618, 13.02991752792604174, 20.00001200000000168 ) ) ;
#2880 = CARTESIAN_POINT ( 'NONE',  ( 32.82842712474624136, 27.17157287525375509, 8.999999999999992895 ) ) ;
#2881 = LINE ( 'NONE', #4629, #4638 ) ;
#2882 = CARTESIAN_POINT ( 'NONE',  ( 2.008133535499844413, 29.93351678898486057, 5.530618255832751018 ) ) ;
#2883 = MANIFOLD_SOLID_BREP ( 'Cut-Extrude7', #4347 ) ;
#2884 = EDGE_CURVE ( 'NONE', #3374, #1902, #1136, .T. ) ;
#2885 = CARTESIAN_POINT ( 'NONE',  ( 0.000000000000000000, 0.000000000000000000, 20.00000000000000000 ) ) ;
#2886 = DIRECTION ( 'NONE',  ( 0.000000000000000000, 0.000000000000000000, -1.000000000000000000 ) ) ;
#2887 = APPLICATION_PROTOCOL_DEFINITION ( 'draft international standard', 'automotive_design', 1998, #335 ) ;
#2888 = AXIS2_PLACEMENT_3D ( 'NONE', #4597, #1341, #577 ) ;
#2889 = MANIFOLD_SOLID_BREP ( 'Boss-Extrude2', #3434 ) ;
#2890 = CARTESIAN_POINT ( 'NONE',  ( 18.21639843360786770, 23.83622240491800426, 8.473444514228560820 ) ) ;
#2891 = LINE ( 'NONE', #1419, #3373 ) ;
#2892 = LINE ( 'NONE', #1797, #971 ) ;
#2893 = PRODUCT_DEFINITION ( 'UNKNOWN', '', #3312, #4290 ) ;
#2894 = ORIENTED_EDGE ( 'NONE', *, *, #3273, .F. ) ;
#2895 = ADVANCED_FACE ( 'NONE', ( #3940 ), #3889, .T. ) ;
#2896 = ORIENTED_EDGE ( 'NONE', *, *, #1043, .T. ) ;
#2897 = ADVANCED_FACE ( 'NONE', ( #1411 ), #3845, .T. ) ;
#2898 = CARTESIAN_POINT ( 'NONE',  ( -3.672066530599461753, 31.77752803659710068, 10.58813356411692830 ) ) ;
#2899 = VECTOR ( 'NONE', #1948, 1000.000000000000114 ) ;
#2900 = CARTESIAN_POINT ( 'NONE',  ( 26.49999999999999645, -0.5000000000000000000, 19.50000000000000000 ) ) ;
#2901 = ORIENTED_EDGE ( 'NONE', *, *, #4060, .F. ) ;
#2902 = EDGE_LOOP ( 'NONE', ( #2, #1119, #1636, #759 ) ) ;
#2903 = VERTEX_POINT ( 'NONE', #591 ) ;
#2904 = CIRCLE ( 'NONE', #852, 5.500000000000000000 ) ;
#2905 = CIRCLE ( 'NONE', #853, 1.750000000000001554 ) ;
#2906 = FACE_BOUND ( 'NONE', #424, .T. ) ;
#2907 = CARTESIAN_POINT ( 'NONE',  ( 3.464101615137757495, 33.00000000000000000, 6.999999999999991118 ) ) ;
#2908 = DIRECTION ( 'NONE',  ( 1.000000000000000000, 0.000000000000000000, 0.000000000000000000 ) ) ;
#2909 = ORIENTED_EDGE ( 'NONE', *, *, #2084, .T. ) ;
#2910 = SURFACE_STYLE_FILL_AREA ( #12 ) ;
#2911 = CARTESIAN_POINT ( 'NONE',  ( 23.34033764136075817, 18.84808613845415337, 11.44520879210846154 ) ) ;
#2912 = APPLICATION_PROTOCOL_DEFINITION ( 'draft international standard', 'automotive_design', 1998, #2446 ) ;
#2913 = CARTESIAN_POINT ( 'NONE',  ( 19.41857644225276402, 22.86845070612086417, 5.819272910265532950 ) ) ;
#2914 = CIRCLE ( 'NONE', #337, 0.5000000000000001110 ) ;
#2915 = DIRECTION ( 'NONE',  ( 0.000000000000000000, 1.000000000000000000, 0.000000000000000000 ) ) ;
#2916 = CARTESIAN_POINT ( 'NONE',  ( -3.464101615137750834, 33.13465464847769937, 6.999999999999991118 ) ) ;
#2917 = EDGE_LOOP ( 'NONE', ( #4444, #2826, #2777, #2337, #327 ) ) ;
#2918 = EDGE_CURVE ( 'NONE', #2120, #3723, #2047, .T. ) ;
#2919 = EDGE_LOOP ( 'NONE', ( #1021, #3951, #4519, #4424 ) ) ;
#2920 = CIRCLE ( 'NONE', #2844, 1.000000000000000000 ) ;
#2921 = DIRECTION ( 'NONE',  ( -0.000000000000000000, -1.000000000000000000, -0.000000000000000000 ) ) ;
#2922 = LINE ( 'NONE', #4374, #3776 ) ;
#2923 = ORIENTED_EDGE ( 'NONE', *, *, #3772, .F. ) ;
#2924 = ORIENTED_EDGE ( 'NONE', *, *, #2152, .F. ) ;
#2925 = EDGE_LOOP ( 'NONE', ( #1835, #1798, #3614, #249 ) ) ;
#2926 = EDGE_CURVE ( 'NONE', #4595, #2849, #2079, .T. ) ;
#2927 = EDGE_CURVE ( 'NONE', #3868, #3995, #2800, .T. ) ;
#2928 = AXIS2_PLACEMENT_3D ( 'NONE', #1780, #1712, #3957 ) ;
#2929 = CARTESIAN_POINT ( 'NONE',  ( 3.469446951953614189E-15, 34.00000000000000000, 8.999999999999992895 ) ) ;
#2930 = CARTESIAN_POINT ( 'NONE',  ( -18.51961241432708505, 23.60157000768430535, 10.77614164618340808 ) ) ;
#2931 = CARTESIAN_POINT ( 'NONE',  ( -13.02991752792603997, -22.56362157461194684, 20.00001200000000168 ) ) ;
#2932 = EDGE_LOOP ( 'NONE', ( #3351, #1719 ) ) ;
#2933 =( GEOMETRIC_REPRESENTATION_CONTEXT ( 3 ) GLOBAL_UNCERTAINTY_ASSIGNED_CONTEXT ( ( #3048 ) ) GLOBAL_UNIT_ASSIGNED_CONTEXT ( ( #1025, #2786, #3256 ) ) REPRESENTATION_CONTEXT ( 'NONE', 'WORKASPACE' ) );
#2934 = VECTOR ( 'NONE', #3367, 1000.000000000000000 ) ;
#2935 = DIRECTION ( 'NONE',  ( -0.000000000000000000, -0.000000000000000000, -1.000000000000000000 ) ) ;
#2936 = VECTOR ( 'NONE', #2977, 1000.000000000000114 ) ;
#2937 = CARTESIAN_POINT ( 'NONE',  ( 8.000000000000000000, 10.00000000000000000, 15.00000000000000178 ) ) ;
#2938 = DIRECTION ( 'NONE',  ( 1.000000000000000000, 0.000000000000000000, 0.000000000000000000 ) ) ;
#2939 = ADVANCED_FACE ( 'NONE', ( #4056 ), #795, .T. ) ;
#2940 = CARTESIAN_POINT ( 'NONE',  ( 23.00034469605617815, 19.26183863435811006, 5.986743120287543185 ) ) ;
#2941 = DIRECTION ( 'NONE',  ( 0.000000000000000000, 0.000000000000000000, 1.000000000000000000 ) ) ;
#2942 = CARTESIAN_POINT ( 'NONE',  ( 0.000000000000000000, 0.000000000000000000, 20.00000000000000000 ) ) ;
#2943 = EDGE_CURVE ( 'NONE', #4217, #895, #1499, .T. ) ;
#2944 = ORIENTED_EDGE ( 'NONE', *, *, #2499, .T. ) ;
#2945 = ORIENTED_EDGE ( 'NONE', *, *, #2839, .T. ) ;
#2946 = CARTESIAN_POINT ( 'NONE',  ( -3.967498225428652159, 31.06568771763734560, 8.474567154859101947 ) ) ;
#2947 = AXIS2_PLACEMENT_3D ( 'NONE', #1310, #4256, #3852 ) ;
#2948 = DIRECTION ( 'NONE',  ( -1.000000000000000000, 0.000000000000000000, 0.000000000000000000 ) ) ;
#2949 = ORIENTED_EDGE ( 'NONE', *, *, #171, .T. ) ;
#2950 = ORIENTED_EDGE ( 'NONE', *, *, #564, .F. ) ;
#2951 = ORIENTED_EDGE ( 'NONE', *, *, #1011, .T. ) ;
#2952 = DIRECTION ( 'NONE',  ( 0.000000000000000000, 1.000000000000000000, -0.000000000000000000 ) ) ;
#2953 = LINE ( 'NONE', #1126, #1606 ) ;
#2954 = CARTESIAN_POINT ( 'NONE',  ( -30.00000000000000355, 0.000000000000000000, 20.00000000000000000 ) ) ;
#2955 = DIRECTION ( 'NONE',  ( 0.000000000000000000, 0.000000000000000000, 1.000000000000000000 ) ) ;
#2956 = PRODUCT_DEFINITION ( 'UNKNOWN', '', #135, #288 ) ;
#2957 = EDGE_LOOP ( 'NONE', ( #622, #3503, #4651, #4497 ) ) ;
#2958 = ADVANCED_FACE ( 'NONE', ( #1454 ), #1476, .T. ) ;
#2959 = AXIS2_PLACEMENT_3D ( 'NONE', #2764, #3818, #1648 ) ;
#2960 = CARTESIAN_POINT ( 'NONE',  ( 3.469446951953614189E-15, 41.00000000000000000, 4.999999999999992006 ) ) ;
#2961 = DIRECTION ( 'NONE',  ( -1.000000000000000000, 0.000000000000000000, 0.000000000000000000 ) ) ;
#2962 = CARTESIAN_POINT ( 'NONE',  ( 21.39894891851820091, 21.02743970908333182, 5.000096751259998307 ) ) ;
#2963 = DIRECTION ( 'NONE',  ( -0.000000000000000000, -0.000000000000000000, -1.000000000000000000 ) ) ;
#2964 = CARTESIAN_POINT ( 'NONE',  ( -3.871991356174924181, 34.73106507380368413, 10.01005989714294842 ) ) ;
#2965 = VERTEX_POINT ( 'NONE', #61 ) ;
#2966 = VERTEX_POINT ( 'NONE', #2960 ) ;
#2967 = CARTESIAN_POINT ( 'NONE',  ( 0.9958591954639605115, 49.00000000000000000, 3.590909090909087276 ) ) ;
#2968 = CARTESIAN_POINT ( 'NONE',  ( 3.469446951953614189E-15, 41.00000000000000000, 8.999999999999992895 ) ) ;
#2969 = VERTEX_POINT ( 'NONE', #4033 ) ;
#2970 = ORIENTED_EDGE ( 'NONE', *, *, #2943, .F. ) ;
#2971 = ORIENTED_EDGE ( 'NONE', *, *, #1520, .T. ) ;
#2972 = UNCERTAINTY_MEASURE_WITH_UNIT (LENGTH_MEASURE( 1.000000000000000082E-05 ), #917, 'distance_accuracy_value', 'NONE');
#2973 = DIRECTION ( 'NONE',  ( 1.000000000000000000, -0.000000000000000000, -0.000000000000000000 ) ) ;
#2974 = DIRECTION ( 'NONE',  ( 0.000000000000000000, 0.000000000000000000, 1.000000000000000000 ) ) ;
#2975 = CYLINDRICAL_SURFACE ( 'NONE', #268, 8.000000000000000000 ) ;
#2976 = MANIFOLD_SOLID_BREP ( 'Sweep1', #1083 ) ;
#2977 = DIRECTION ( 'NONE',  ( 8.659560562354903276E-17, -0.7071067811865500152, 0.7071067811865451302 ) ) ;
#2978 = VECTOR ( 'NONE', #755, 1000.000000000000000 ) ;
#2979 = ORIENTED_EDGE ( 'NONE', *, *, #1999, .F. ) ;
#2980 = DIRECTION ( 'NONE',  ( 0.000000000000000000, 0.000000000000000000, -1.000000000000000000 ) ) ;
#2981 = CIRCLE ( 'NONE', #4210, 1.500000000000000222 ) ;
#2982 = LINE ( 'NONE', #2261, #3000 ) ;
#2983 = EDGE_CURVE ( 'NONE', #834, #1543, #1433, .T. ) ;
#2984 = ADVANCED_FACE ( 'NONE', ( #774 ), #3690, .T. ) ;
#2985 = CARTESIAN_POINT ( 'NONE',  ( 21.93593546006599126, 20.46659425767087015, 5.128325996195414405 ) ) ;
#2986 = DIRECTION ( 'NONE',  ( 0.000000000000000000, 0.000000000000000000, -1.000000000000000000 ) ) ;
#2987 = PLANE ( 'NONE',  #2171 ) ;
#2988 = ORIENTED_EDGE ( 'NONE', *, *, #91, .T. ) ;
#2989 = ORIENTED_EDGE ( 'NONE', *, *, #199, .T. ) ;
#2990 = CARTESIAN_POINT ( 'NONE',  ( -3.464101615137752166, 32.86760366373215447, 10.99999999999999822 ) ) ;
#2991 = DIRECTION ( 'NONE',  ( 0.000000000000000000, -0.000000000000000000, 1.000000000000000000 ) ) ;
#2992 = SURFACE_SIDE_STYLE ('',( #473 ) ) ;
#2993 = DIRECTION ( 'NONE',  ( 0.000000000000000000, 0.000000000000000000, 1.000000000000000000 ) ) ;
#2994 = EDGE_LOOP ( 'NONE', ( #3252, #1422, #3567, #408 ) ) ;
#2995 = VERTEX_POINT ( 'NONE', #1789 ) ;
#2996 = VERTEX_POINT ( 'NONE', #3337 ) ;
#2997 = ORIENTED_EDGE ( 'NONE', *, *, #3593, .F. ) ;
#2998 = DIRECTION ( 'NONE',  ( 0.000000000000000000, 0.000000000000000000, 1.000000000000000000 ) ) ;
#2999 = CARTESIAN_POINT ( 'NONE',  ( -23.52581488222647010, 18.61605759292307383, 11.00403192580902711 ) ) ;
#3000 = VECTOR ( 'NONE', #3363, 1000.000000000000000 ) ;
#3001 = EDGE_CURVE ( 'NONE', #4496, #3310, #87, .T. ) ;
#3002 = SURFACE_STYLE_FILL_AREA ( #815 ) ;
#3003 = ORIENTED_EDGE ( 'NONE', *, *, #2029, .T. ) ;
#3004 = VECTOR ( 'NONE', #2641, 1000.000000000000000 ) ;
#3005 = CARTESIAN_POINT ( 'NONE',  ( 0.5000000000000001110, 10.00000000000000000, 13.00000000000000178 ) ) ;
#3006 = CARTESIAN_POINT ( 'NONE',  ( 3.471741185006992136, 32.73575814869636957, 10.98693824102217853 ) ) ;
#3007 = COLOUR_RGB ( '',0.8941176470588234615, 0.8941176470588234615, 0.8941176470588234615 ) ;
#3008 = ADVANCED_FACE ( 'NONE', ( #1525 ), #1082, .F. ) ;
#3009 = AXIS2_PLACEMENT_3D ( 'NONE', #3824, #1282, #2771 ) ;
#3010 =( REPRESENTATION_RELATIONSHIP ('NONE','NONE', #2397, #773 ) REPRESENTATION_RELATIONSHIP_WITH_TRANSFORMATION ( #3987 )SHAPE_REPRESENTATION_RELATIONSHIP( ) );
#3011 = CARTESIAN_POINT ( 'NONE',  ( 4.081770351527290718E-15, 34.00000000000000000, 13.99999999999999467 ) ) ;
#3012 = DIRECTION ( 'NONE',  ( 0.000000000000000000, 1.000000000000000000, 0.000000000000000000 ) ) ;
#3013 = ADVANCED_FACE ( 'NONE', ( #4434 ), #2496, .T. ) ;
#3014 = ORIENTED_EDGE ( 'NONE', *, *, #3698, .F. ) ;
#3015 = CARTESIAN_POINT ( 'NONE',  ( 25.99519186311192342, 0.5000000000000000000, 19.00000000000000000 ) ) ;
#3016 = CARTESIAN_POINT ( 'NONE',  ( -25.99519186311192342, 0.5000000000000000000, 19.00000000000000000 ) ) ;
#3017 = CARTESIAN_POINT ( 'NONE',  ( 0.000000000000000000, 0.000000000000000000, 0.000000000000000000 ) ) ;
#3018 = CARTESIAN_POINT ( 'NONE',  ( 3.959305671612554781E-15, 37.00000000000000711, 12.99999999999999289 ) ) ;
#3019 = ORIENTED_EDGE ( 'NONE', *, *, #2927, .F. ) ;
#3020 = ORIENTED_EDGE ( 'NONE', *, *, #4137, .T. ) ;
#3021 = ORIENTED_EDGE ( 'NONE', *, *, #1110, .T. ) ;
#3022 = ORIENTED_EDGE ( 'NONE', *, *, #3074, .F. ) ;
#3023 = DIRECTION ( 'NONE',  ( 1.000000000000000000, 0.000000000000000000, 0.000000000000000000 ) ) ;
#3024 = CARTESIAN_POINT ( 'NONE',  ( 13.74999999999999822, 45.00000000000000000, 0.000000000000000000 ) ) ;
#3025 = PLANE ( 'NONE',  #4686 ) ;
#3026 = CIRCLE ( 'NONE', #1732, 5.500000000000000000 ) ;
#3027 = LINE ( 'NONE', #701, #1509 ) ;
#3028 = LINE ( 'NONE', #3362, #707 ) ;
#3029 = AXIS2_PLACEMENT_3D ( 'NONE', #1316, #4220, #2092 ) ;
#3030 = DIRECTION ( 'NONE',  ( 1.000000000000000000, -0.000000000000000000, -0.000000000000000000 ) ) ;
#3031 = ITEM_DEFINED_TRANSFORMATION ( 'NONE', 'NONE', #2545,  #2928 ) ;
#3032 = AXIS2_PLACEMENT_3D ( 'NONE', #1985, #4132, #3842 ) ;
#3033 = MANIFOLD_SOLID_BREP ( 'Cut-Extrude2', #1991 ) ;
#3034 = FACE_OUTER_BOUND ( 'NONE', #2743, .T. ) ;
#3035 = CARTESIAN_POINT ( 'NONE',  ( -3.464101615137749057, 33.13263078466293621, 10.99999999999999289 ) ) ;
#3036 = DIRECTION ( 'NONE',  ( 0.000000000000000000, 1.000000000000000000, 0.000000000000000000 ) ) ;
#3037 = CARTESIAN_POINT ( 'NONE',  ( 0.7500000000000000000, -2.999999999999999556, 18.19999999999999929 ) ) ;
#3038 = DIRECTION ( 'NONE',  ( 0.000000000000000000, -0.000000000000000000, 1.000000000000000000 ) ) ;
#3039 = ORIENTED_EDGE ( 'NONE', *, *, #2355, .T. ) ;
#3040 = AXIS2_PLACEMENT_3D ( 'NONE', #25, #2921, #760 ) ;
#3041 = EDGE_CURVE ( 'NONE', #4199, #2657, #989, .T. ) ;
#3042 = ORIENTED_EDGE ( 'NONE', *, *, #1524, .T. ) ;
#3043 = EDGE_LOOP ( 'NONE', ( #3064, #1858, #2005, #3839, #3189, #1193, #1956, #1162 ) ) ;
#3044 = ADVANCED_FACE ( 'NONE', ( #893, #2347 ), #535, .T. ) ;
#3045 = ORIENTED_EDGE ( 'NONE', *, *, #1399, .T. ) ;
#3046 = DIRECTION ( 'NONE',  ( 1.982541115402063335E-15, 1.000000000000000000, 0.000000000000000000 ) ) ;
#3047 = LINE ( 'NONE', #4575, #463 ) ;
#3048 = UNCERTAINTY_MEASURE_WITH_UNIT (LENGTH_MEASURE( 1.000000000000000082E-05 ), #1025, 'distance_accuracy_value', 'NONE');
#3049 = DIRECTION ( 'NONE',  ( 0.000000000000000000, 0.000000000000000000, 1.000000000000000000 ) ) ;
#3050 = SHAPE_REPRESENTATION ( 'glass', ( #2928 ), #1184 ) ;
#3051 = PRODUCT_DEFINITION_SHAPE ( 'NONE', 'NONE',  #3648 ) ;
#3052 = ORIENTED_EDGE ( 'NONE', *, *, #2213, .F. ) ;
#3053 = CARTESIAN_POINT ( 'NONE',  ( 3.469446951953614189E-15, 25.00000000000000000, 8.999999999999992895 ) ) ;
#3054 = CARTESIAN_POINT ( 'NONE',  ( 25.99307600111999150, -0.5999999999999996447, 19.59999999999999787 ) ) ;
#3055 = DIRECTION ( 'NONE',  ( 0.000000000000000000, 1.000000000000000000, 0.000000000000000000 ) ) ;
#3056 = ORIENTED_EDGE ( 'NONE', *, *, #1661, .T. ) ;
#3057 = AXIS2_PLACEMENT_3D ( 'NONE', #224, #4628, #988 ) ;
#3058 = FACE_OUTER_BOUND ( 'NONE', #4632, .T. ) ;
#3059 = DIRECTION ( 'NONE',  ( 0.000000000000000000, 0.000000000000000000, -1.000000000000000000 ) ) ;
#3060 = DIRECTION ( 'NONE',  ( 0.000000000000000000, 0.000000000000000000, 1.000000000000000000 ) ) ;
#3061 = CARTESIAN_POINT ( 'NONE',  ( 3.877033663942015984, 34.74339188317524219, 7.985269980068071760 ) ) ;
#3062 = CARTESIAN_POINT ( 'NONE',  ( 0.000000000000000000, 0.000000000000000000, 0.000000000000000000 ) ) ;
#3063 = CARTESIAN_POINT ( 'NONE',  ( 4.081770351527290718E-15, 39.99999999999999289, 13.99999999999999289 ) ) ;
#3064 = ORIENTED_EDGE ( 'NONE', *, *, #1260, .F. ) ;
#3065 = ADVANCED_FACE ( 'NONE', ( #4486 ), #4206, .T. ) ;
#3066 = ORIENTED_EDGE ( 'NONE', *, *, #3909, .F. ) ;
#3067 = ORIENTED_EDGE ( 'NONE', *, *, #2238, .T. ) ;
#3068 = ORIENTED_EDGE ( 'NONE', *, *, #3215, .T. ) ;
#3069 = CARTESIAN_POINT ( 'NONE',  ( 30.00000000000005684, 29.99999999999995026, 8.999999999999992895 ) ) ;
#3070 = CARTESIAN_POINT ( 'NONE',  ( -0.5000000000000000000, 0.8660254037844387076, 20.00000000000000000 ) ) ;
#3071 = ADVANCED_FACE ( 'NONE', ( #1325 ), #4185, .T. ) ;
#3072 = VECTOR ( 'NONE', #733, 1000.000000000000000 ) ;
#3073 = CARTESIAN_POINT ( 'NONE',  ( 3.469446951953614189E-15, 34.00000000000000000, 13.99999999999999289 ) ) ;
#3074 = EDGE_CURVE ( 'NONE', #2707, #1614, #1301, .T. ) ;
#3075 = EDGE_LOOP ( 'NONE', ( #1686, #3227, #1827, #2604 ) ) ;
#3076 = AXIS2_PLACEMENT_3D ( 'NONE', #4011, #2190, #4388 ) ;
#3077 = LINE ( 'NONE', #110, #3278 ) ;
#3078 = CARTESIAN_POINT ( 'NONE',  ( 3.469446951953614189E-15, 49.00000000000000000, 8.999999999999992895 ) ) ;
#3079 = DIRECTION ( 'NONE',  ( 0.000000000000000000, -1.000000000000000000, 0.000000000000000000 ) ) ;
#3080 = ORIENTED_EDGE ( 'NONE', *, *, #2078, .F. ) ;
#3081 = DIRECTION ( 'NONE',  ( -1.927470528863123239E-16, 1.000000000000000000, 0.000000000000000000 ) ) ;
#3082 = CARTESIAN_POINT ( 'NONE',  ( 3.469446951953614189E-15, 40.00000000000000000, 8.999999999999992895 ) ) ;
#3083 = CIRCLE ( 'NONE', #2097, 1.249999999999999334 ) ;
#3084 = CARTESIAN_POINT ( 'NONE',  ( 0.7500000000000000000, -2.999999999999999556, 17.69999999999999929 ) ) ;
#3085 = CYLINDRICAL_SURFACE ( 'NONE', #4026, 3.999999999999998224 ) ;
#3086 = EDGE_CURVE ( 'NONE', #1737, #477, #511, .T. ) ;
#3087 = DIRECTION ( 'NONE',  ( 1.000000000000000000, 0.000000000000000000, 0.000000000000000000 ) ) ;
#3088 = AXIS2_PLACEMENT_3D ( 'NONE', #2703, #2729, #4169 ) ;
#3089 = AXIS2_PLACEMENT_3D ( 'NONE', #541, #1990, #183 ) ;
#3090 = LINE ( 'NONE', #998, #2673 ) ;
#3091 = ORIENTED_EDGE ( 'NONE', *, *, #1935, .T. ) ;
#3092 = EDGE_LOOP ( 'NONE', ( #2642, #2988, #1995, #526 ) ) ;
#3093 = EDGE_CURVE ( 'NONE', #2276, #525, #3871, .T. ) ;
#3094 = ORIENTED_EDGE ( 'NONE', *, *, #230, .F. ) ;
#3095 = ORIENTED_EDGE ( 'NONE', *, *, #1308, .F. ) ;
#3096 = FACE_BOUND ( 'NONE', #4097, .T. ) ;
#3097 = FACE_OUTER_BOUND ( 'NONE', #787, .T. ) ;
#3098 = DIRECTION ( 'NONE',  ( 1.982541115402063335E-15, 1.000000000000000000, 0.000000000000000000 ) ) ;
#3099 = ORIENTED_EDGE ( 'NONE', *, *, #1650, .F. ) ;
#3100 = LINE ( 'NONE', #2346, #1834 ) ;
#3101 = DIRECTION ( 'NONE',  ( 0.000000000000000000, 0.000000000000000000, 1.000000000000000000 ) ) ;
#3102 = AXIS2_PLACEMENT_3D ( 'NONE', #2052, #2493, #1347 ) ;
#3103 = DIRECTION ( 'NONE',  ( -0.000000000000000000, -0.000000000000000000, 1.000000000000000000 ) ) ;
#3104 = ADVANCED_FACE ( 'NONE', ( #1225 ), #202, .T. ) ;
#3105 = ORIENTED_EDGE ( 'NONE', *, *, #3093, .F. ) ;
#3106 = EDGE_CURVE ( 'NONE', #289, #181, #2869, .T. ) ;
#3107 = CIRCLE ( 'NONE', #4321, 4.000000000000000000 ) ;
#3108 = ADVANCED_FACE ( 'NONE', ( #2398 ), #3767, .T. ) ;
#3109 = CARTESIAN_POINT ( 'NONE',  ( 20.46667490424620084, 21.93582988124910216, 12.87153294081770483 ) ) ;
#3110 =( GEOMETRIC_REPRESENTATION_CONTEXT ( 3 ) GLOBAL_UNCERTAINTY_ASSIGNED_CONTEXT ( ( #1879 ) ) GLOBAL_UNIT_ASSIGNED_CONTEXT ( ( #2838, #2817, #657 ) ) REPRESENTATION_CONTEXT ( 'NONE', 'WORKASPACE' ) );
#3111 = CARTESIAN_POINT ( 'NONE',  ( -27.10000000000000497, 0.6000000000000000888, 19.00000000000000000 ) ) ;
#3112 = AXIS2_PLACEMENT_3D ( 'NONE', #3158, #4215, #2775 ) ;
#3113 = CARTESIAN_POINT ( 'NONE',  ( 0.5000000000000000000, 0.8660254037844387076, 20.00000000000000000 ) ) ;
#3114 = CARTESIAN_POINT ( 'NONE',  ( -20.50609665440989815, 14.84924240491747227, 8.999999999999992895 ) ) ;
#3115 = DIRECTION ( 'NONE',  ( 0.000000000000000000, 1.000000000000000000, 0.000000000000000000 ) ) ;
#3116 = VERTEX_POINT ( 'NONE', #3054 ) ;
#3117 = AXIS2_PLACEMENT_3D ( 'NONE', #266, #290, #1783 ) ;
#3118 = ORIENTED_EDGE ( 'NONE', *, *, #2632, .T. ) ;
#3119 = VERTEX_POINT ( 'NONE', #559 ) ;
#3120 = LINE ( 'NONE', #3878, #1662 ) ;
#3121 = DIRECTION ( 'NONE',  ( -1.000000000000000000, 0.000000000000000000, 0.000000000000000000 ) ) ;
#3122 = DIRECTION ( 'NONE',  ( 1.000000000000000000, -1.621111868633889227E-15, 0.000000000000000000 ) ) ;
#3123 = DIRECTION ( 'NONE',  ( 0.000000000000000000, 1.000000000000000000, 0.000000000000000000 ) ) ;
#3124 = LINE ( 'NONE', #3522, #4050 ) ;
#3125 = LINE ( 'NONE', #2692, #118 ) ;
#3126 = ORIENTED_EDGE ( 'NONE', *, *, #727, .T. ) ;
#3127 = ADVANCED_FACE ( 'NONE', ( #4509 ), #1253, .T. ) ;
#3128 = AXIS2_PLACEMENT_3D ( 'NONE', #2299, #2321, #2003 ) ;
#3129 = CARTESIAN_POINT ( 'NONE',  ( -3.999903055931597784, 29.73215053696358368, 8.737301635141733414 ) ) ;
#3130 = ADVANCED_FACE ( 'NONE', ( #3797 ), #1624, .T. ) ;
#3131 = DIRECTION ( 'NONE',  ( 1.000000000000000000, 0.000000000000000000, 0.000000000000000000 ) ) ;
#3132 = EDGE_CURVE ( 'NONE', #4134, #2995, #245, .T. ) ;
#3133 = CIRCLE ( 'NONE', #1157, 1.000000000000000000 ) ;
#3134 = DIRECTION ( 'NONE',  ( 1.000000000000000000, -0.000000000000000000, 0.000000000000000000 ) ) ;
#3135 = DIRECTION ( 'NONE',  ( -1.000000000000000000, 0.000000000000000000, 0.000000000000000000 ) ) ;
#3136 = DIRECTION ( 'NONE',  ( 1.000000000000000000, 0.000000000000000000, 0.000000000000000000 ) ) ;
#3137 = ORIENTED_EDGE ( 'NONE', *, *, #2329, .F. ) ;
#3138 = VECTOR ( 'NONE', #3213, 1000.000000000000000 ) ;
#3139 = ORIENTED_EDGE ( 'NONE', *, *, #2690, .T. ) ;
#3140 = ORIENTED_EDGE ( 'NONE', *, *, #688, .T. ) ;
#3141 = DIRECTION ( 'NONE',  ( 0.000000000000000000, 0.000000000000000000, 1.000000000000000000 ) ) ;
#3142 = PLANE ( 'NONE',  #3128 ) ;
#3143 = CARTESIAN_POINT ( 'NONE',  ( 3.469446951953614189E-15, 25.00000000000000000, 8.999999999999992895 ) ) ;
#3144 = CARTESIAN_POINT ( 'NONE',  ( 2.255140518769849223E-14, 49.00000000000000000, 3.499999999999992895 ) ) ;
#3145 = CYLINDRICAL_SURFACE ( 'NONE', #1534, 1.000000000000000888 ) ;
#3146 = EDGE_CURVE ( 'NONE', #3799, #1195, #821, .T. ) ;
#3147 = AXIS2_PLACEMENT_3D ( 'NONE', #2153, #4015, #2868 ) ;
#3148 = DIRECTION ( 'NONE',  ( -0.000000000000000000, -0.000000000000000000, -1.000000000000000000 ) ) ;
#3149 = CARTESIAN_POINT ( 'NONE',  ( 2.255140518769849223E-14, 37.00000000000000000, 3.499999999999992895 ) ) ;
#3150 = ORIENTED_EDGE ( 'NONE', *, *, #3132, .T. ) ;
#3151 = CIRCLE ( 'NONE', #4366, 0.5000000000000000000 ) ;
#3152 = DIRECTION ( 'NONE',  ( 0.000000000000000000, 0.000000000000000000, -1.000000000000000000 ) ) ;
#3153 = CIRCLE ( 'NONE', #190, 1.500000000000000222 ) ;
#3154 = DIRECTION ( 'NONE',  ( -0.000000000000000000, -0.000000000000000000, 1.000000000000000000 ) ) ;
#3155 = DIRECTION ( 'NONE',  ( 0.000000000000000000, 0.000000000000000000, 1.000000000000000000 ) ) ;
#3156 = VECTOR ( 'NONE', #1962, 1000.000000000000000 ) ;
#3157 = CARTESIAN_POINT ( 'NONE',  ( 0.000000000000000000, 0.000000000000000000, 17.69999999999999929 ) ) ;
#3158 = CARTESIAN_POINT ( 'NONE',  ( 0.000000000000000000, 0.000000000000000000, 17.69999999999999929 ) ) ;
#3159 = DIRECTION ( 'NONE',  ( 0.000000000000000000, 1.000000000000000000, -0.000000000000000000 ) ) ;
#3160 = EDGE_CURVE ( 'NONE', #3353, #803, #2124, .T. ) ;
#3161 = COLOUR_RGB ( '',0.8941176470588234615, 0.8941176470588234615, 0.8941176470588234615 ) ;
#3162 = AXIS2_PLACEMENT_3D ( 'NONE', #2242, #3696, #1894 ) ;
#3163 = EDGE_LOOP ( 'NONE', ( #3260, #1350, #4144, #1289 ) ) ;
#3164 = ORIENTED_EDGE ( 'NONE', *, *, #1556, .T. ) ;
#3165 = CARTESIAN_POINT ( 'NONE',  ( 0.7500000000000001110, 9.184850993605150903E-17, 18.19999999999999929 ) ) ;
#3166 = VECTOR ( 'NONE', #4677, 1000.000000000000000 ) ;
#3167 = PLANE ( 'NONE',  #2424 ) ;
#3168 = AXIS2_PLACEMENT_3D ( 'NONE', #4023, #3657, #4332 ) ;
#3169 = CARTESIAN_POINT ( 'NONE',  ( 25.83240171513483929, 3.403349963601484340, 20.00001200000000168 ) ) ;
#3170 = DIRECTION ( 'NONE',  ( -1.000000000000000000, 0.000000000000000000, 0.000000000000000000 ) ) ;
#3171 = CARTESIAN_POINT ( 'NONE',  ( 0.000000000000000000, 0.000000000000000000, 20.00000000000000000 ) ) ;
#3172 = DIRECTION ( 'NONE',  ( 0.000000000000000000, 0.000000000000000000, -1.000000000000000000 ) ) ;
#3173 = ORIENTED_EDGE ( 'NONE', *, *, #1240, .F. ) ;
#3174 = LINE ( 'NONE', #3196, #2614 ) ;
#3175 = DIRECTION ( 'NONE',  ( -0.000000000000000000, -1.000000000000000000, -0.000000000000000000 ) ) ;
#3176 = AXIS2_PLACEMENT_3D ( 'NONE', #4546, #1663, #261 ) ;
#3177 = CARTESIAN_POINT ( 'NONE',  ( -0.7500000000000000000, -2.999999999999999556, 17.69999999999999929 ) ) ;
#3178 = AXIS2_PLACEMENT_3D ( 'NONE', #3469, #2043, #547 ) ;
#3179 = AXIS2_PLACEMENT_3D ( 'NONE', #4010, #3264, #3241 ) ;
#3180 = CYLINDRICAL_SURFACE ( 'NONE', #184, 4.000000000000000000 ) ;
#3181 = CARTESIAN_POINT ( 'NONE',  ( -3.672900200782970526, 34.23223752615971449, 7.403954086897937437 ) ) ;
#3182 = VERTEX_POINT ( 'NONE', #1741 ) ;
#3183 = ORIENTED_EDGE ( 'NONE', *, *, #3267, .T. ) ;
#3184 = AXIS2_PLACEMENT_3D ( 'NONE', #1694, #2790, #3884 ) ;
#3185 = CARTESIAN_POINT ( 'NONE',  ( -25.99307600111999150, 0.6000000000000000888, 20.00001200000000168 ) ) ;
#3186 = CARTESIAN_POINT ( 'NONE',  ( 4.081770351527290718E-15, 41.00000000000000000, 13.99999999999999289 ) ) ;
#3187 =( NAMED_UNIT ( * ) PLANE_ANGLE_UNIT ( ) SI_UNIT ( $, .RADIAN. ) );
#3188 = EDGE_CURVE ( 'NONE', #2608, #1930, #63, .T. ) ;
#3189 = ORIENTED_EDGE ( 'NONE', *, *, #2811, .T. ) ;
#3190 = CARTESIAN_POINT ( 'NONE',  ( -0.5000000000000001110, 10.00000000000000000, 15.00000000000000178 ) ) ;
#3191 = APPLICATION_CONTEXT ( 'automotive_design' ) ;
#3192 = CARTESIAN_POINT ( 'NONE',  ( 3.469446951953614189E-15, 37.00000000000000711, 8.999999999999992895 ) ) ;
#3193 = DIRECTION ( 'NONE',  ( 5.782411586589374402E-16, -1.000000000000000000, 0.000000000000000000 ) ) ;
#3194 = CARTESIAN_POINT ( 'NONE',  ( 3.469446951953614189E-15, 41.00000000000000000, 8.999999999999992895 ) ) ;
#3195 =( LENGTH_UNIT ( ) NAMED_UNIT ( * ) SI_UNIT ( .MILLI., .METRE. ) );
#3196 = CARTESIAN_POINT ( 'NONE',  ( -26.50000000000000355, 0.5000000000000000000, 19.50000000000000000 ) ) ;
#3197 = APPLICATION_PROTOCOL_DEFINITION ( 'draft international standard', 'automotive_design', 1998, #422 ) ;
#3198 = CARTESIAN_POINT ( 'NONE',  ( 26.00000000000000355, 1.592040838891558898E-15, 20.00000599999999906 ) ) ;
#3199 = CARTESIAN_POINT ( 'NONE',  ( -23.83622240491805755, 18.21639843360778244, 8.473444514228551938 ) ) ;
#3200 = CARTESIAN_POINT ( 'NONE',  ( 27.99999999999999645, 3.551475717527324030E-15, 20.00000000000000000 ) ) ;
#3201 = PLANE ( 'NONE',  #3236 ) ;
#3202 = AXIS2_PLACEMENT_3D ( 'NONE', #3157, #4255, #3223 ) ;
#3203 = ORIENTED_EDGE ( 'NONE', *, *, #745, .F. ) ;
#3204 = VERTEX_POINT ( 'NONE', #4604 ) ;
#3205 = VECTOR ( 'NONE', #844, 1000.000000000000000 ) ;
#3206 = DIRECTION ( 'NONE',  ( -1.000000000000000000, 0.000000000000000000, -0.000000000000000000 ) ) ;
#3207 = EDGE_CURVE ( 'NONE', #3445, #3995, #2881, .T. ) ;
#3208 =( NAMED_UNIT ( * ) SI_UNIT ( $, .STERADIAN. ) SOLID_ANGLE_UNIT ( ) );
#3209 = DIRECTION ( 'NONE',  ( -0.000000000000000000, -1.000000000000000000, -0.000000000000000000 ) ) ;
#3210 = DIRECTION ( 'NONE',  ( 0.000000000000000000, 0.000000000000000000, 1.000000000000000000 ) ) ;
#3211 = ADVANCED_FACE ( 'NONE', ( #4246 ), #4337, .T. ) ;
#3212 = ORIENTED_EDGE ( 'NONE', *, *, #229, .T. ) ;
#3213 = DIRECTION ( 'NONE',  ( 0.000000000000000000, -1.000000000000000000, 0.000000000000000000 ) ) ;
#3214 = DIRECTION ( 'NONE',  ( -0.7071067811865487940, 0.7071067811865463515, 0.000000000000000000 ) ) ;
#3215 = EDGE_CURVE ( 'NONE', #2731, #741, #703, .T. ) ;
#3216 = CARTESIAN_POINT ( 'NONE',  ( 26.49999999999999645, 0.5000000000000000000, 19.50000000000000000 ) ) ;
#3217 = EDGE_CURVE ( 'NONE', #27, #3324, #2835, .T. ) ;
#3218 = CARTESIAN_POINT ( 'NONE',  ( 2.004043995866382932, 29.93378982679665512, 12.47171604645195941 ) ) ;
#3219 = CARTESIAN_POINT ( 'NONE',  ( 4.000043395258034096, 30.99991320946996964, 9.131973577465631209 ) ) ;
#3220 = APPLICATION_PROTOCOL_DEFINITION ( 'draft international standard', 'automotive_design', 1998, #3191 ) ;
#3221 = VECTOR ( 'NONE', #3081, 1000.000000000000000 ) ;
#3222 = AXIS2_PLACEMENT_3D ( 'NONE', #462, #3667, #4110 ) ;
#3223 = DIRECTION ( 'NONE',  ( 1.000000000000000000, 0.000000000000000000, 0.000000000000000000 ) ) ;
#3224 = DIRECTION ( 'NONE',  ( 0.000000000000000000, 0.000000000000000000, 1.000000000000000000 ) ) ;
#3225 = DIRECTION ( 'NONE',  ( -0.000000000000000000, -1.000000000000000000, 0.000000000000000000 ) ) ;
#3226 = CIRCLE ( 'NONE', #1178, 13.75000000000000000 ) ;
#3227 = ORIENTED_EDGE ( 'NONE', *, *, #2078, .T. ) ;
#3228 = ORIENTED_EDGE ( 'NONE', *, *, #1404, .F. ) ;
#3229 = SURFACE_STYLE_USAGE ( .BOTH. , #4262 ) ;
#3230 =( NAMED_UNIT ( * ) SI_UNIT ( $, .STERADIAN. ) SOLID_ANGLE_UNIT ( ) );
#3231 = SURFACE_STYLE_USAGE ( .BOTH. , #265 ) ;
#3232 = CARTESIAN_POINT ( 'NONE',  ( 8.999999999999980460, 32.99999999999999289, 0.000000000000000000 ) ) ;
#3233 = ADVANCED_FACE ( 'NONE', ( #1365 ), #3906, .T. ) ;
#3234 = EDGE_LOOP ( 'NONE', ( #3755, #836, #1885, #3613, #376 ) ) ;
#3235 = DIRECTION ( 'NONE',  ( -1.000000000000000000, 0.000000000000000000, -3.469446951953614189E-15 ) ) ;
#3236 = AXIS2_PLACEMENT_3D ( 'NONE', #1773, #2176, #1115 ) ;
#3237 = DIRECTION ( 'NONE',  ( 0.000000000000000000, 0.000000000000000000, 1.000000000000000000 ) ) ;
#3238 = CARTESIAN_POINT ( 'NONE',  ( 3.469446951953614189E-15, 37.00000000000000000, 8.999999999999992895 ) ) ;
#3239 = DIRECTION ( 'NONE',  ( -1.000000000000000000, 0.000000000000000000, 0.000000000000000000 ) ) ;
#3240 = COLOUR_RGB ( '',0.8941176470588234615, 0.8941176470588234615, 0.8941176470588234615 ) ;
#3241 = DIRECTION ( 'NONE',  ( 0.000000000000000000, 0.000000000000000000, -1.000000000000000000 ) ) ;
#3242 = ADVANCED_FACE ( 'NONE', ( #2099 ), #1765, .T. ) ;
#3243 = DIRECTION ( 'NONE',  ( 0.000000000000000000, 1.000000000000000000, 0.000000000000000000 ) ) ;
#3244 = APPLICATION_PROTOCOL_DEFINITION ( 'draft international standard', 'automotive_design', 1998, #3583 ) ;
#3245 = EDGE_CURVE ( 'NONE', #4522, #4217, #2568, .T. ) ;
#3246 = EDGE_CURVE ( 'NONE', #1643, #3829, #532, .T. ) ;
#3247 = CARTESIAN_POINT ( 'NONE',  ( 0.7500000000000000000, -2.999999999999999556, 18.19999999999999929 ) ) ;
#3248 = FACE_OUTER_BOUND ( 'NONE', #4333, .T. ) ;
#3249 = CIRCLE ( 'NONE', #1202, 1.750000000000001554 ) ;
#3250 = DIRECTION ( 'NONE',  ( -0.000000000000000000, -0.000000000000000000, 1.000000000000000000 ) ) ;
#3251 =( REPRESENTATION_RELATIONSHIP ('NONE','NONE', #2397, #3382 ) REPRESENTATION_RELATIONSHIP_WITH_TRANSFORMATION ( #2521 )SHAPE_REPRESENTATION_RELATIONSHIP( ) );
#3252 = ORIENTED_EDGE ( 'NONE', *, *, #538, .T. ) ;
#3253 = VERTEX_POINT ( 'NONE', #1409 ) ;
#3254 = MECHANICAL_DESIGN_GEOMETRIC_PRESENTATION_REPRESENTATION (  '', ( #754 ), #3331 ) ;
#3255 = SURFACE_STYLE_FILL_AREA ( #3900 ) ;
#3256 =( NAMED_UNIT ( * ) SI_UNIT ( $, .STERADIAN. ) SOLID_ANGLE_UNIT ( ) );
#3257 = DIRECTION ( 'NONE',  ( -0.000000000000000000, 1.000000000000000000, -0.000000000000000000 ) ) ;
#3258 = VERTEX_POINT ( 'NONE', #1032 ) ;
#3259 = ORIENTED_EDGE ( 'NONE', *, *, #778, .T. ) ;
#3260 = ORIENTED_EDGE ( 'NONE', *, *, #2839, .F. ) ;
#3261 = CARTESIAN_POINT ( 'NONE',  ( 0.5000000000000000000, 0.000000000000000000, 19.50000000000000000 ) ) ;
#3262 = CARTESIAN_POINT ( 'NONE',  ( -3.889087296526001047, 34.17157287525380838, 5.110912703473974084 ) ) ;
#3263 = CARTESIAN_POINT ( 'NONE',  ( -12.00000000000000178, 36.00000000000001421, 0.000000000000000000 ) ) ;
#3264 = DIRECTION ( 'NONE',  ( -0.000000000000000000, -1.000000000000000000, -0.000000000000000000 ) ) ;
#3265 = CARTESIAN_POINT ( 'NONE',  ( 3.948285692887626652, 31.10501000327115761, 9.652966208173760165 ) ) ;
#3266 = SHAPE_DEFINITION_REPRESENTATION ( #4274, #2397 ) ;
#3267 = EDGE_CURVE ( 'NONE', #2680, #2090, #2039, .T. ) ;
#3268 =( GEOMETRIC_REPRESENTATION_CONTEXT ( 3 ) GLOBAL_UNCERTAINTY_ASSIGNED_CONTEXT ( ( #837 ) ) GLOBAL_UNIT_ASSIGNED_CONTEXT ( ( #4288, #2071, #3953 ) ) REPRESENTATION_CONTEXT ( 'NONE', 'WORKASPACE' ) );
#3269 = CARTESIAN_POINT ( 'NONE',  ( 22.10738654751468957, 20.28106296843835565, 5.205249767788495241 ) ) ;
#3270 = DIRECTION ( 'NONE',  ( 1.000000000000000000, 0.000000000000000000, 0.000000000000000000 ) ) ;
#3271 = EDGE_CURVE ( 'NONE', #377, #2686, #2859, .T. ) ;
#3272 = CARTESIAN_POINT ( 'NONE',  ( -0.9958591954639913757, 49.00000000000000000, 14.40909090909089230 ) ) ;
#3273 = EDGE_CURVE ( 'NONE', #2091, #4272, #3952, .T. ) ;
#3274 = ORIENTED_EDGE ( 'NONE', *, *, #613, .F. ) ;
#3275 = ORIENTED_EDGE ( 'NONE', *, *, #2605, .F. ) ;
#3276 = CARTESIAN_POINT ( 'NONE',  ( -3.606676218660104016, 31.99081763496160136, 7.268492701228250752 ) ) ;
#3277 = VECTOR ( 'NONE', #4648, 1000.000000000000000 ) ;
#3278 = VECTOR ( 'NONE', #534, 1000.000000000000000 ) ;
#3279 = DIRECTION ( 'NONE',  ( 8.921435019309286191E-15, 1.000000000000000000, 0.000000000000000000 ) ) ;
#3280 = EDGE_LOOP ( 'NONE', ( #443, #524, #4080, #2364 ) ) ;
#3281 = ORIENTED_EDGE ( 'NONE', *, *, #3595, .T. ) ;
#3282 = ORIENTED_EDGE ( 'NONE', *, *, #3848, .T. ) ;
#3283 = AXIS2_PLACEMENT_3D ( 'NONE', #1669, #1323, #3904 ) ;
#3284 = LINE ( 'NONE', #2880, #360 ) ;
#3285 = CARTESIAN_POINT ( 'NONE',  ( -23.34243530581964166, 18.84548434425186869, 11.44084376890924304 ) ) ;
#3286 = DIRECTION ( 'NONE',  ( 0.000000000000000000, 0.000000000000000000, 1.000000000000000000 ) ) ;
#3287 = ADVANCED_FACE ( 'NONE', ( #4704 ), #3501, .T. ) ;
#3288 = ORIENTED_EDGE ( 'NONE', *, *, #2715, .T. ) ;
#3289 = LINE ( 'NONE', #1478, #872 ) ;
#3290 = ITEM_DEFINED_TRANSFORMATION ( 'NONE', 'NONE', #3927,  #2928 ) ;
#3291 = CARTESIAN_POINT ( 'NONE',  ( 20.46703030200860240, 21.93550942649225632, 5.128274502689554204 ) ) ;
#3292 = AXIS2_PLACEMENT_3D ( 'NONE', #4364, #640, #3913 ) ;
#3293 = CARTESIAN_POINT ( 'NONE',  ( 3.469446951953614189E-15, 30.00000000000000355, 4.999999999999992006 ) ) ;
#3294 = CARTESIAN_POINT ( 'NONE',  ( 3.464101615137757495, 33.00000000000000000, 6.999999999999991118 ) ) ;
#3295 = ORIENTED_EDGE ( 'NONE', *, *, #3595, .F. ) ;
#3297 = VERTEX_POINT ( 'NONE', #633 ) ;
#3296 = ADVANCED_BREP_SHAPE_REPRESENTATION ( '', ( #4442, #2928 ), #2543 ) ;
#3298 = CARTESIAN_POINT ( 'NONE',  ( -4.000056596598882130, 30.99988680677069297, 8.869325943800758338 ) ) ;
#3299 = ADVANCED_FACE ( 'NONE', ( #2075 ), #3546, .T. ) ;
#3300 =( LENGTH_UNIT ( ) NAMED_UNIT ( * ) SI_UNIT ( .MILLI., .METRE. ) );
#3301 = CIRCLE ( 'NONE', #3912, 4.000000000000000000 ) ;
#3302 = FACE_OUTER_BOUND ( 'NONE', #1421, .T. ) ;
#3303 = VERTEX_POINT ( 'NONE', #3016 ) ;
#3304 = ADVANCED_FACE ( 'NONE', ( #4493 ), #2517, .F. ) ;
#3305 = ORIENTED_EDGE ( 'NONE', *, *, #4413, .T. ) ;
#3306 = ORIENTED_EDGE ( 'NONE', *, *, #1306, .F. ) ;
#3307 = CARTESIAN_POINT ( 'NONE',  ( -20.84186778456427902, 21.57966755480311960, 12.97440020260208193 ) ) ;
#3308 = DIRECTION ( 'NONE',  ( 1.000000000000000000, 0.000000000000000000, 0.000000000000000000 ) ) ;
#3309 = CARTESIAN_POINT ( 'NONE',  ( -23.36965697125209473, -11.52193136556785547, 20.00001200000000523 ) ) ;
#3310 = VERTEX_POINT ( 'NONE', #521 ) ;
#3311 = AXIS2_PLACEMENT_3D ( 'NONE', #4306, #714, #1753 ) ;
#3312 = PRODUCT_DEFINITION_FORMATION_WITH_SPECIFIED_SOURCE ( 'ANY', '', #3390, .NOT_KNOWN. ) ;
#3313 = AXIS2_PLACEMENT_3D ( 'NONE', #3082, #1474, #661 ) ;
#3314 = DIRECTION ( 'NONE',  ( 0.7071067811865487940, -0.7071067811865463515, 0.000000000000000000 ) ) ;
#3315 = CARTESIAN_POINT ( 'NONE',  ( 4.528983652092238188, 49.00000000000000000, 5.879373928346857348 ) ) ;
#3316 = CARTESIAN_POINT ( 'NONE',  ( 2.255140518769849223E-14, 34.17157287525380838, 3.499999999999992895 ) ) ;
#3317 = DIRECTION ( 'NONE',  ( 1.000000000000000000, 0.000000000000000000, 0.000000000000000000 ) ) ;
#3318 = ORIENTED_EDGE ( 'NONE', *, *, #363, .F. ) ;
#3319 = B_SPLINE_CURVE_WITH_KNOTS ( 'NONE', 3,
 ( #2154, #2916, #3993, #3534, #734, #1728, #3181, #4644, #1374, #2824, #1019, #4393, #2625, #116, #3671, #391, #4418, #1160, #2964, #4089, #825, #441, #3721, #2195, #1231, #1558, #3035, #1865 ),
 .UNSPECIFIED., .F., .F.,
 ( 4, 2, 2, 2, 2, 2, 2, 2, 2, 2, 2, 2, 2, 4 ),
 ( 0.000000000000000000, 0.0003975746136738172597, 0.0007951492273476345194, 0.001590298454695269689, 0.002385447682042904968, 0.002783022295716721956, 0.003180596909390539379, 0.003578171523064356801, 0.003975746136738173356, 0.004373320750411991212, 0.004770895364085809068, 0.005566044591433457790, 0.005963619205107282585, 0.006361193818781107380 ),
 .UNSPECIFIED. ) ;
#3320 = ORIENTED_EDGE ( 'NONE', *, *, #2715, .F. ) ;
#3321 = DIRECTION ( 'NONE',  ( 0.000000000000000000, 0.000000000000000000, 1.000000000000000000 ) ) ;
#3322 = AXIS2_PLACEMENT_3D ( 'NONE', #3411, #158, #1599 ) ;
#3323 = DIRECTION ( 'NONE',  ( 0.000000000000000000, -0.000000000000000000, 1.000000000000000000 ) ) ;
#3324 = VERTEX_POINT ( 'NONE', #3037 ) ;
#3325 = ORIENTED_EDGE ( 'NONE', *, *, #3578, .F. ) ;
#3326 = ORIENTED_EDGE ( 'NONE', *, *, #4639, .T. ) ;
#3327 = CIRCLE ( 'NONE', #4549, 5.500000000000000000 ) ;
#3328 = DIRECTION ( 'NONE',  ( -0.7071067811865487940, -0.7071067811865463515, 0.000000000000000000 ) ) ;
#3329 = CARTESIAN_POINT ( 'NONE',  ( -22.43321928693951506, 19.92007681871555036, 12.59316242105108508 ) ) ;
#3330 = EDGE_CURVE ( 'NONE', #4217, #4522, #1062, .T. ) ;
#3331 =( GEOMETRIC_REPRESENTATION_CONTEXT ( 3 ) GLOBAL_UNCERTAINTY_ASSIGNED_CONTEXT ( ( #3354 ) ) GLOBAL_UNIT_ASSIGNED_CONTEXT ( ( #3195, #3485, #2471 ) ) REPRESENTATION_CONTEXT ( 'NONE', 'WORKASPACE' ) );
#3332 = DIRECTION ( 'NONE',  ( -0.000000000000000000, -1.000000000000000000, -0.000000000000000000 ) ) ;
#3333 = CARTESIAN_POINT ( 'NONE',  ( 11.52193136556785369, -23.36965697125208052, 20.00001199999999457 ) ) ;
#3334 = EDGE_CURVE ( 'NONE', #1199, #574, #963, .T. ) ;
#3335 = VERTEX_POINT ( 'NONE', #2539 ) ;
#3336 = AXIS2_PLACEMENT_3D ( 'NONE', #1286, #927, #3441 ) ;
#3337 = CARTESIAN_POINT ( 'NONE',  ( -26.50000000000000355, -0.5000000000000000000, 19.50000000000000000 ) ) ;
#3338 = CARTESIAN_POINT ( 'NONE',  ( -3.120626071653210154, 37.00000000000000000, 13.52898365209217246 ) ) ;
#3339 = AXIS2_PLACEMENT_3D ( 'NONE', #4540, #1657, #3513 ) ;
#3340 = CARTESIAN_POINT ( 'NONE',  ( 19.74756467586676223, 22.58496929628982031, 5.529782636833618703 ) ) ;
#3341 = CARTESIAN_POINT ( 'NONE',  ( 0.000000000000000000, 10.00000000000000000, 17.00000000000000000 ) ) ;
#3342 = CARTESIAN_POINT ( 'NONE',  ( 0.9958591954638856825, 43.00000000000000000, 14.40909090909091361 ) ) ;
#3343 = VERTEX_POINT ( 'NONE', #3703 ) ;
#3344 = CIRCLE ( 'NONE', #2578, 4.749999999999999112 ) ;
#3345 = EDGE_LOOP ( 'NONE', ( #238, #2872, #4573, #1844 ) ) ;
#3346 = DIRECTION ( 'NONE',  ( 0.000000000000000000, 0.000000000000000000, 1.000000000000000000 ) ) ;
#3347 = CARTESIAN_POINT ( 'NONE',  ( 5.409090909090912724, 49.00000000000000000, 8.004140804536053366 ) ) ;
#3348 = FILL_AREA_STYLE_COLOUR ( '', #3161 ) ;
#3349 = CARTESIAN_POINT ( 'NONE',  ( -25.99307600111999150, 0.5999999999999998668, 19.00000000000000000 ) ) ;
#3350 = EDGE_LOOP ( 'NONE', ( #2046, #450, #1242, #1173 ) ) ;
#3351 = ORIENTED_EDGE ( 'NONE', *, *, #2837, .T. ) ;
#3352 = ORIENTED_EDGE ( 'NONE', *, *, #2646, .T. ) ;
#3353 = VERTEX_POINT ( 'NONE', #4006 ) ;
#3354 = UNCERTAINTY_MEASURE_WITH_UNIT (LENGTH_MEASURE( 1.000000000000000082E-05 ), #3195, 'distance_accuracy_value', 'NONE');
#3355 = AXIS2_PLACEMENT_3D ( 'NONE', #3701, #3321, #1537 ) ;
#3356 = CARTESIAN_POINT ( 'NONE',  ( 3.469446951953614189E-15, 49.00000000000000000, 8.999999999999992895 ) ) ;
#3357 = CARTESIAN_POINT ( 'NONE',  ( 3.469446951953614189E-15, 34.00000000000000000, 8.999999999999992895 ) ) ;
#3358 = ADVANCED_FACE ( 'NONE', ( #806 ), #4472, .T. ) ;
#3359 = CARTESIAN_POINT ( 'NONE',  ( -26.00000000000000355, -1.592040838891558504E-15, 20.00000599999999906 ) ) ;
#3360 = VECTOR ( 'NONE', #3365, 1000.000000000000000 ) ;
#3361 = VERTEX_POINT ( 'NONE', #1210 ) ;
#3362 = CARTESIAN_POINT ( 'NONE',  ( 30.00000000000000355, 3.673940397442059967E-15, 20.00000000000000000 ) ) ;
#3363 = DIRECTION ( 'NONE',  ( -1.000000000000000000, 0.000000000000000000, 0.000000000000000000 ) ) ;
#3364 = AXIS2_PLACEMENT_3D ( 'NONE', #3568, #2417, #676 ) ;
#3365 = DIRECTION ( 'NONE',  ( -1.000000000000000000, 0.000000000000000000, 0.000000000000000000 ) ) ;
#3366 = CARTESIAN_POINT ( 'NONE',  ( -8.999999999999973355, 32.99999999999999289, 0.000000000000000000 ) ) ;
#3367 = DIRECTION ( 'NONE',  ( 0.000000000000000000, 0.000000000000000000, -1.000000000000000000 ) ) ;
#3368 = ORIENTED_EDGE ( 'NONE', *, *, #4269, .T. ) ;
#3369 = CARTESIAN_POINT ( 'NONE',  ( -3.464101615137750390, 33.00000000000000000, 10.99999999999999467 ) ) ;
#3370 = CARTESIAN_POINT ( 'NONE',  ( 3.464101615137757495, 33.13441662254499676, 6.999999999999990230 ) ) ;
#3371 = CARTESIAN_POINT ( 'NONE',  ( 3.889087296525981063, 34.17157287525380838, 12.88908729652603746 ) ) ;
#3372 = ORIENTED_EDGE ( 'NONE', *, *, #2449, .T. ) ;
#3373 = VECTOR ( 'NONE', #4324, 1000.000000000000000 ) ;
#3374 = VERTEX_POINT ( 'NONE', #3347 ) ;
#3375 = ORIENTED_EDGE ( 'NONE', *, *, #1260, .T. ) ;
#3376 = ORIENTED_EDGE ( 'NONE', *, *, #4465, .T. ) ;
#3377 = DIRECTION ( 'NONE',  ( 0.000000000000000000, 0.000000000000000000, 1.000000000000000000 ) ) ;
#3378 = CARTESIAN_POINT ( 'NONE',  ( 3.469446951953614189E-15, 34.00000000000000000, 8.999999999999992895 ) ) ;
#3379 = CONICAL_SURFACE ( 'NONE', #1337, 4.000000000000000000, 0.7853981633974447263 ) ;
#3380 = PRODUCT_DEFINITION_CONTEXT ( 'detailed design', #3583, 'design' ) ;
#3381 = DIRECTION ( 'NONE',  ( 0.000000000000000000, 1.000000000000000000, 0.000000000000000000 ) ) ;
#3382 = SHAPE_REPRESENTATION ( 'start button', ( #2928 ), #3388 ) ;
#3383 = ORIENTED_EDGE ( 'NONE', *, *, #3939, .F. ) ;
#3384 = VECTOR ( 'NONE', #4528, 1000.000000000000114 ) ;
#3385 = CYLINDRICAL_SURFACE ( 'NONE', #1390, 0.5000000000000001110 ) ;
#3386 = DIRECTION ( 'NONE',  ( 0.000000000000000000, -1.000000000000000000, 0.000000000000000000 ) ) ;
#3387 = CARTESIAN_POINT ( 'NONE',  ( -30.00000000000004974, 29.99999999999995737, 8.999999999999992895 ) ) ;
#3388 =( GEOMETRIC_REPRESENTATION_CONTEXT ( 3 ) GLOBAL_UNCERTAINTY_ASSIGNED_CONTEXT ( ( #4455 ) ) GLOBAL_UNIT_ASSIGNED_CONTEXT ( ( #1961, #2342, #604 ) ) REPRESENTATION_CONTEXT ( 'NONE', 'WORKASPACE' ) );
#3389 = AXIS2_PLACEMENT_3D ( 'NONE', #1605, #1259, #1331 ) ;
#3390 = PRODUCT ( 'second hand', 'second hand', '', ( #3646 ) ) ;
#3391 = MECHANICAL_DESIGN_GEOMETRIC_PRESENTATION_REPRESENTATION (  '', ( #4696 ), #4310 ) ;
#3392 = EDGE_CURVE ( 'NONE', #2577, #895, #4561, .T. ) ;
#3393 = EDGE_CURVE ( 'NONE', #2111, #2552, #3726, .T. ) ;
#3394 = CYLINDRICAL_SURFACE ( 'NONE', #566, 1.500000000000000222 ) ;
#3395 = EDGE_CURVE ( 'NONE', #1485, #377, #3702, .T. ) ;
#3396 = CARTESIAN_POINT ( 'NONE',  ( 3.469446951953614189E-15, 37.00000000000000711, 8.999999999999992895 ) ) ;
#3397 = ORIENTED_EDGE ( 'NONE', *, *, #3741, .F. ) ;
#3398 = CARTESIAN_POINT ( 'NONE',  ( -8.999999999999976907, 31.24999999999999645, 0.000000000000000000 ) ) ;
#3399 = DIRECTION ( 'NONE',  ( 1.000000000000000000, 0.000000000000000000, 0.000000000000000000 ) ) ;
#3400 = PLANE ( 'NONE',  #4571 ) ;
#3401 = ORIENTED_EDGE ( 'NONE', *, *, #1725, .T. ) ;
#3402 = VERTEX_POINT ( 'NONE', #851 ) ;
#3403 = EDGE_LOOP ( 'NONE', ( #2233, #1535, #1977, #2779 ) ) ;
#3404 = ORIENTED_EDGE ( 'NONE', *, *, #987, .T. ) ;
#3405 = DIRECTION ( 'NONE',  ( -0.7071067811865487940, -0.7071067811865463515, 0.000000000000000000 ) ) ;
#3406 = CARTESIAN_POINT ( 'NONE',  ( 3.959305671612554781E-15, 25.00000000000000000, 12.99999999999999289 ) ) ;
#3407 = CARTESIAN_POINT ( 'NONE',  ( -0.7500000000000000000, -1.299038105676658450, 17.69999999999999929 ) ) ;
#3408 = CARTESIAN_POINT ( 'NONE',  ( -27.10000000000000497, -0.5999999999999998668, 19.59999999999999787 ) ) ;
#3409 = CARTESIAN_POINT ( 'NONE',  ( 0.000000000000000000, 0.000000000000000000, 20.00000000000000000 ) ) ;
#3410 = VECTOR ( 'NONE', #2935, 1000.000000000000000 ) ;
#3411 = CARTESIAN_POINT ( 'NONE',  ( 3.469446951953614189E-15, 49.00000000000000000, 8.999999999999992895 ) ) ;
#3412 = DIRECTION ( 'NONE',  ( 0.000000000000000000, 0.000000000000000000, 1.000000000000000000 ) ) ;
#3413 = ORIENTED_EDGE ( 'NONE', *, *, #2510, .F. ) ;
#3414 = ADVANCED_FACE ( 'NONE', ( #256 ), #1680, .T. ) ;
#3415 = AXIS2_PLACEMENT_3D ( 'NONE', #889, #3123, #2051 ) ;
#3416 = CARTESIAN_POINT ( 'NONE',  ( 19.41770456673556922, 22.86919556969938583, 12.17989986600643704 ) ) ;
#3417 = CARTESIAN_POINT ( 'NONE',  ( -3.889087296526001047, 49.00000000000000000, 5.110912703473974084 ) ) ;
#3418 = EDGE_CURVE ( 'NONE', #4371, #3687, #2123, .T. ) ;
#3419 = CARTESIAN_POINT ( 'NONE',  ( -18.84457784187181062, 23.34316218245334795, 6.560806493199571321 ) ) ;
#3420 = DIRECTION ( 'NONE',  ( -0.000000000000000000, 1.000000000000000000, -0.000000000000000000 ) ) ;
#3421 = EDGE_CURVE ( 'NONE', #715, #788, #677, .T. ) ;
#3422 = SURFACE_STYLE_FILL_AREA ( #2819 ) ;
#3423 = CARTESIAN_POINT ( 'NONE',  ( 0.000000000000000000, 0.000000000000000000, 19.50000000000000000 ) ) ;
#3424 = ORIENTED_EDGE ( 'NONE', *, *, #3709, .T. ) ;
#3425 = ORIENTED_EDGE ( 'NONE', *, *, #91, .F. ) ;
#3426 = ORIENTED_EDGE ( 'NONE', *, *, #3888, .F. ) ;
#3427 = ORIENTED_EDGE ( 'NONE', *, *, #751, .F. ) ;
#3428 = CARTESIAN_POINT ( 'NONE',  ( -12.00000000000000178, 44.99999999999999289, 0.000000000000000000 ) ) ;
#3429 = FACE_OUTER_BOUND ( 'NONE', #4543, .T. ) ;
#3430 = ORIENTED_EDGE ( 'NONE', *, *, #309, .F. ) ;
#3431 = DIRECTION ( 'NONE',  ( 0.000000000000000000, 1.000000000000000000, 0.000000000000000000 ) ) ;
#3432 = EDGE_CURVE ( 'NONE', #3258, #2385, #77, .T. ) ;
#3433 = LINE ( 'NONE', #180, #2769 ) ;
#3434 = CLOSED_SHELL ( 'NONE', ( #3633, #2280, #3211, #1361, #1788, #1091, #3242, #960, #3452, #425, #620, #896 ) ) ;
#3435 = ORIENTED_EDGE ( 'NONE', *, *, #2413, .F. ) ;
#3436 = AXIS2_PLACEMENT_3D ( 'NONE', #3053, #3431, #4083 ) ;
#3437 = ADVANCED_FACE ( 'NONE', ( #2334 ), #3085, .F. ) ;
#3438 = CARTESIAN_POINT ( 'NONE',  ( 3.959305739469038251E-15, 30.00000000000000355, 12.99999999999999289 ) ) ;
#3439 = CARTESIAN_POINT ( 'NONE',  ( 3.469446951953614189E-15, 37.00000000000000000, 8.999999999999992895 ) ) ;
#3440 = CARTESIAN_POINT ( 'NONE',  ( -26.00000000000000711, 0.000000000000000000, 19.50000000000000000 ) ) ;
#3441 = DIRECTION ( 'NONE',  ( -1.000000000000000000, 0.000000000000000000, 0.000000000000000000 ) ) ;
#3442 =( LENGTH_UNIT ( ) NAMED_UNIT ( * ) SI_UNIT ( .MILLI., .METRE. ) );
#3443 = CARTESIAN_POINT ( 'NONE',  ( -3.120626071653146649, 37.00000000000000000, 4.471016347907768029 ) ) ;
#3444 = ORIENTED_EDGE ( 'NONE', *, *, #2837, .F. ) ;
#3445 = VERTEX_POINT ( 'NONE', #4235 ) ;
#3446 = ORIENTED_EDGE ( 'NONE', *, *, #2191, .T. ) ;
#3447 = ORIENTED_EDGE ( 'NONE', *, *, #1249, .F. ) ;
#3448 = DIRECTION ( 'NONE',  ( -0.000000000000000000, -1.000000000000000000, -0.000000000000000000 ) ) ;
#3449 = PRODUCT_RELATED_PRODUCT_CATEGORY ( 'part', '', ( #507 ) ) ;
#3450 =( NAMED_UNIT ( * ) SI_UNIT ( $, .STERADIAN. ) SOLID_ANGLE_UNIT ( ) );
#3451 = SHAPE_REPRESENTATION_RELATIONSHIP ( 'NONE' , 'NONE' ,  #3382, #1996 ) ;
#3452 = ADVANCED_FACE ( 'NONE', ( #3807 ), #2042, .T. ) ;
#3453 = AXIS2_PLACEMENT_3D ( 'NONE', #1230, #65, #2309 ) ;
#3454 = CARTESIAN_POINT ( 'NONE',  ( -8.999999999999973355, 32.99999999999999289, 0.000000000000000000 ) ) ;
#3455 = DIRECTION ( 'NONE',  ( 1.000000000000000000, 0.000000000000000000, 0.000000000000000000 ) ) ;
#3456 = CIRCLE ( 'NONE', #1401, 1.749999999999999778 ) ;
#3457 = EDGE_CURVE ( 'NONE', #2196, #29, #218, .T. ) ;
#3458 = DIRECTION ( 'NONE',  ( 0.000000000000000000, 1.000000000000000000, 0.000000000000000000 ) ) ;
#3459 = DIRECTION ( 'NONE',  ( 0.000000000000000000, 0.000000000000000000, 1.000000000000000000 ) ) ;
#3460 = FACE_OUTER_BOUND ( 'NONE', #548, .T. ) ;
#3461 = ORIENTED_EDGE ( 'NONE', *, *, #2581, .F. ) ;
#3462=STYLED_ITEM('',(#4729),#4442);
#3463 = CARTESIAN_POINT ( 'NONE',  ( -4.000096396247766251, 29.73212452601126188, 9.259737768674039415 ) ) ;
#3464 = DIRECTION ( 'NONE',  ( 0.000000000000000000, 1.000000000000000000, 0.000000000000000000 ) ) ;
#3465 =( GEOMETRIC_REPRESENTATION_CONTEXT ( 3 ) GLOBAL_UNCERTAINTY_ASSIGNED_CONTEXT ( ( #4482 ) ) GLOBAL_UNIT_ASSIGNED_CONTEXT ( ( #3954, #1050, #3208 ) ) REPRESENTATION_CONTEXT ( 'NONE', 'WORKASPACE' ) );
#3466 = AXIS2_PLACEMENT_3D ( 'NONE', #3439, #1678, #4611 ) ;
#3467 = CARTESIAN_POINT ( 'NONE',  ( 3.469446951953614189E-15, 25.00000000000000000, 8.999999999999992895 ) ) ;
#3468 = DIRECTION ( 'NONE',  ( -0.000000000000000000, -1.000000000000000000, -0.000000000000000000 ) ) ;
#3469 = CARTESIAN_POINT ( 'NONE',  ( 0.000000000000000000, 0.000000000000000000, 19.00000000000000000 ) ) ;
#3470 = ORIENTED_EDGE ( 'NONE', *, *, #924, .F. ) ;
#3471 = EDGE_LOOP ( 'NONE', ( #500, #1589, #513, #1255 ) ) ;
#3472 = VERTEX_POINT ( 'NONE', #977 ) ;
#3473 = ORIENTED_EDGE ( 'NONE', *, *, #2214, .F. ) ;
#3474 = FACE_OUTER_BOUND ( 'NONE', #239, .T. ) ;
#3475 = CARTESIAN_POINT ( 'NONE',  ( 10.24999999999999822, 45.00000000000000000, 2.143131898507898126E-16 ) ) ;
#3476 = DIRECTION ( 'NONE',  ( 1.000000000000000000, 0.000000000000000000, 0.000000000000000000 ) ) ;
#3477 = VERTEX_POINT ( 'NONE', #3512 ) ;
#3478 = EDGE_LOOP ( 'NONE', ( #2677, #2525, #1303, #2506, #1123, #3320, #192, #355, #2458 ) ) ;
#3479 = CARTESIAN_POINT ( 'NONE',  ( 5.409090909090912724, 43.00000000000000000, 9.995859195463930646 ) ) ;
#3480 = EDGE_CURVE ( 'NONE', #1614, #1896, #279, .T. ) ;
#3481 = DIRECTION ( 'NONE',  ( 1.000000000000000000, 0.000000000000000000, 0.000000000000000000 ) ) ;
#3482 = ADVANCED_FACE ( 'NONE', ( #3533 ), #1972, .T. ) ;
#3483 = ORIENTED_EDGE ( 'NONE', *, *, #281, .T. ) ;
#3484 = CIRCLE ( 'NONE', #3866, 0.9999999999999991118 ) ;
#3485 =( NAMED_UNIT ( * ) PLANE_ANGLE_UNIT ( ) SI_UNIT ( $, .RADIAN. ) );
#3486 = CYLINDRICAL_SURFACE ( 'NONE', #870, 1.000000000000000000 ) ;
#3487 = MECHANICAL_DESIGN_GEOMETRIC_PRESENTATION_REPRESENTATION (  '', ( #606 ), #3110 ) ;
#3488 = CARTESIAN_POINT ( 'NONE',  ( -0.7500000000000001110, 1.299038105676658450, 18.19999999999999929 ) ) ;
#3489 = CARTESIAN_POINT ( 'NONE',  ( -22.10500230410275790, 20.28368189782978703, 5.203924605526645486 ) ) ;
#3490 = CARTESIAN_POINT ( 'NONE',  ( 0.000000000000000000, 0.000000000000000000, 15.00000000000000178 ) ) ;
#3491 = CARTESIAN_POINT ( 'NONE',  ( 0.000000000000000000, 0.000000000000000000, 0.000000000000000000 ) ) ;
#3492 = VERTEX_POINT ( 'NONE', #2801 ) ;
#3493 = ORIENTED_EDGE ( 'NONE', *, *, #469, .F. ) ;
#3494 = VERTEX_POINT ( 'NONE', #3114 ) ;
#3495 = EDGE_CURVE ( 'NONE', #2996, #2297, #2407, .T. ) ;
#3496 = FACE_OUTER_BOUND ( 'NONE', #3280, .T. ) ;
#3497 = FILL_AREA_STYLE ('',( #3789 ) ) ;
#3498 = APPLICATION_CONTEXT ( 'automotive_design' ) ;
#3499 = DIRECTION ( 'NONE',  ( -0.7071067811865484609, 0.000000000000000000, 0.7071067811865467956 ) ) ;
#3500 = CARTESIAN_POINT ( 'NONE',  ( 0.000000000000000000, 0.000000000000000000, 17.69999999999999929 ) ) ;
#3501 = CYLINDRICAL_SURFACE ( 'NONE', #3184, 5.000000000000000888 ) ;
#3502 = LINE ( 'NONE', #4582, #1855 ) ;
#3503 = ORIENTED_EDGE ( 'NONE', *, *, #3577, .T. ) ;
#3504 = CARTESIAN_POINT ( 'NONE',  ( 8.999999999999980460, 32.99999999999999289, 0.000000000000000000 ) ) ;
#3505 = PRODUCT_DEFINITION_SHAPE ( 'NONE', 'NONE',  #839 ) ;
#3506 = AXIS2_PLACEMENT_3D ( 'NONE', #2158, #2116, #4 ) ;
#3507 = PRODUCT_DEFINITION ( 'UNKNOWN', '', #2033, #4626 ) ;
#3508 = DIRECTION ( 'NONE',  ( 0.000000000000000000, 1.000000000000000000, 0.000000000000000000 ) ) ;
#3509 = DIRECTION ( 'NONE',  ( -0.000000000000000000, 1.000000000000000000, -0.000000000000000000 ) ) ;
#3510 = AXIS2_PLACEMENT_3D ( 'NONE', #3378, #403, #130 ) ;
#3511 = CARTESIAN_POINT ( 'NONE',  ( -23.60249532755124591, 18.51843501006184312, 7.226626843687534496 ) ) ;
#3512 = CARTESIAN_POINT ( 'NONE',  ( -24.00000000000000355, 2.939152317953648289E-15, 19.00000000000000000 ) ) ;
#3513 = DIRECTION ( 'NONE',  ( 1.000000000000000000, 0.000000000000000000, 0.000000000000000000 ) ) ;
#3514 = VERTEX_POINT ( 'NONE', #3874 ) ;
#3515 = VERTEX_POINT ( 'NONE', #2728 ) ;
#3516 = CYLINDRICAL_SURFACE ( 'NONE', #3176, 1.749999999999999778 ) ;
#3517 = CARTESIAN_POINT ( 'NONE',  ( -4.528983652092254175, 49.00000000000000000, 12.12062607165309558 ) ) ;
#3518 =( LENGTH_UNIT ( ) NAMED_UNIT ( * ) SI_UNIT ( .MILLI., .METRE. ) );
#3519 = PRODUCT_DEFINITION_CONTEXT ( 'detailed design', #3836, 'design' ) ;
#3520 = CARTESIAN_POINT ( 'NONE',  ( 1.701696020694463574, 25.99999999999999645, 20.00001200000000168 ) ) ;
#3521 =( REPRESENTATION_RELATIONSHIP ('NONE','NONE', #2397, #1408 ) REPRESENTATION_RELATIONSHIP_WITH_TRANSFORMATION ( #2150 )SHAPE_REPRESENTATION_RELATIONSHIP( ) );
#3522 = CARTESIAN_POINT ( 'NONE',  ( -32.82842712474623426, 27.17157287525376219, 8.999999999999992895 ) ) ;
#3523 = CIRCLE ( 'NONE', #1467, 1.000000000000000000 ) ;
#3524 = DIRECTION ( 'NONE',  ( 1.000000000000000000, 0.000000000000000000, -0.000000000000000000 ) ) ;
#3525 = CARTESIAN_POINT ( 'NONE',  ( 4.000183053129181765, 29.73211286767113037, 8.738350868772759128 ) ) ;
#3526 = ORIENTED_EDGE ( 'NONE', *, *, #4622, .F. ) ;
#3527 = CIRCLE ( 'NONE', #1779, 0.5000000000000001110 ) ;
#3528 = CIRCLE ( 'NONE', #122, 30.00000000000000355 ) ;
#3529 = CARTESIAN_POINT ( 'NONE',  ( 23.85222316637486273, 18.19536891688240843, 8.999999999999992895 ) ) ;
#3530 = CARTESIAN_POINT ( 'NONE',  ( -23.85222316637485562, 18.19536891688241198, 8.999999999999992895 ) ) ;
#3531 = EDGE_CURVE ( 'NONE', #4376, #2044, #2492, .T. ) ;
#3532 = EDGE_CURVE ( 'NONE', #763, #460, #4329, .T. ) ;
#3533 = FACE_OUTER_BOUND ( 'NONE', #588, .T. ) ;
#3534 = CARTESIAN_POINT ( 'NONE',  ( -3.501309621998935917, 33.52503659006909942, 7.065645527993494213 ) ) ;
#3535 =( GEOMETRIC_REPRESENTATION_CONTEXT ( 3 ) GLOBAL_UNCERTAINTY_ASSIGNED_CONTEXT ( ( #860 ) ) GLOBAL_UNIT_ASSIGNED_CONTEXT ( ( #447, #2269, #2529 ) ) REPRESENTATION_CONTEXT ( 'NONE', 'WORKASPACE' ) );
#3536 = VECTOR ( 'NONE', #163, 1000.000000000000000 ) ;
#3537 = B_SPLINE_CURVE_WITH_KNOTS ( 'NONE', 3,
 ( #2836, #271, #4705, #315, #295, #4248, #3218, #2147, #1742, #3964, #1389, #2100, #991, #4657, #3885, #4296, #2421, #3525, #2860, #704, #634, #3547, #1033, #2518, #2442, #2791, #339, #2882, #4681, #4631, #1009, #2125, #2814, #1348 ),
 .UNSPECIFIED., .F., .F.,
 ( 4, 2, 2, 2, 2, 2, 2, 2, 2, 2, 2, 2, 2, 2, 2, 2, 4 ),
 ( 0.01251976117704806969, 0.01330205745918825073, 0.01408435374132843351, 0.01486665002346861456, 0.01564894630560879560, 0.01643124258774897664, 0.01721353886988916115, 0.01799583515202934220, 0.01877813143416952324, 0.01956042771630970428, 0.02034272399844988533, 0.02112502028059006637, 0.02190731656273024741, 0.02268961284487042845, 0.02347190912701060950, 0.02425420540915079401, 0.02503650169129097505 ),
 .UNSPECIFIED. ) ;
#3538 = ORIENTED_EDGE ( 'NONE', *, *, #84, .T. ) ;
#3539 = ORIENTED_EDGE ( 'NONE', *, *, #2605, .T. ) ;
#3540 = CARTESIAN_POINT ( 'NONE',  ( 17.67766952966372429, 17.67766952966365679, 8.999999999999992895 ) ) ;
#3541 = CIRCLE ( 'NONE', #3313, 5.000000000000002665 ) ;
#3542 = FACE_OUTER_BOUND ( 'NONE', #1498, .T. ) ;
#3543 = EDGE_LOOP ( 'NONE', ( #2198, #2949, #272, #1729 ) ) ;
#3544 = CARTESIAN_POINT ( 'NONE',  ( -27.10000000000000497, -0.5999999999999998668, 19.59999999999999787 ) ) ;
#3545 = CYLINDRICAL_SURFACE ( 'NONE', #1837, 26.00000000000000711 ) ;
#3546 = PLANE ( 'NONE',  #1054 ) ;
#3547 = CARTESIAN_POINT ( 'NONE',  ( 3.595673326866945629, 29.78391060080977226, 7.228055294346797943 ) ) ;
#3548 = FILL_AREA_STYLE_COLOUR ( '', #609 ) ;
#3549 = VECTOR ( 'NONE', #679, 1000.000000000000000 ) ;
#3550 = CARTESIAN_POINT ( 'NONE',  ( 3.464101615137757495, 33.00000000000000000, 6.999999999999991118 ) ) ;
#3551 = CARTESIAN_POINT ( 'NONE',  ( 8.377607117416804527, -24.67207871933483787, 20.00001200000000168 ) ) ;
#3552 = CIRCLE ( 'NONE', #1057, 10.25000000000000000 ) ;
#3553 = EDGE_CURVE ( 'NONE', #3494, #2903, #3669, .T. ) ;
#3554 = DIRECTION ( 'NONE',  ( 0.7071067811865487940, 0.7071067811865463515, 0.000000000000000000 ) ) ;
#3555 = DIRECTION ( 'NONE',  ( -0.000000000000000000, 1.000000000000000000, 0.000000000000000000 ) ) ;
#3556 = CYLINDRICAL_SURFACE ( 'NONE', #421, 8.000000000000000000 ) ;
#3557 = ADVANCED_FACE ( 'NONE', ( #2428 ), #3180, .T. ) ;
#3558 = EDGE_LOOP ( 'NONE', ( #452, #2709, #3832, #1405 ) ) ;
#3559 = ORIENTED_EDGE ( 'NONE', *, *, #2083, .F. ) ;
#3560 = AXIS2_PLACEMENT_3D ( 'NONE', #4448, #1187, #3399 ) ;
#3561 = EDGE_CURVE ( 'NONE', #4272, #1877, #1022, .T. ) ;
#3562 = CYLINDRICAL_SURFACE ( 'NONE', #3796, 0.9999999999999991118 ) ;
#3563 = FACE_OUTER_BOUND ( 'NONE', #2434, .T. ) ;
#3564 = AXIS2_PLACEMENT_3D ( 'NONE', #1322, #2762, #3499 ) ;
#3565 = CARTESIAN_POINT ( 'NONE',  ( 0.5000000000000000000, 0.000000000000000000, 19.50000000000000000 ) ) ;
#3566 = LINE ( 'NONE', #1051, #277 ) ;
#3567 = ORIENTED_EDGE ( 'NONE', *, *, #4242, .T. ) ;
#3568 = CARTESIAN_POINT ( 'NONE',  ( 0.000000000000000000, 0.000000000000000000, 19.50000000000000000 ) ) ;
#3569 = CARTESIAN_POINT ( 'NONE',  ( -0.7500000000000001110, 9.184850993605150903E-17, 17.00000000000000000 ) ) ;
#3570 = CARTESIAN_POINT ( 'NONE',  ( 0.5000000000000000000, -0.8660254037844387076, 19.50000000000000000 ) ) ;
#3571 = CARTESIAN_POINT ( 'NONE',  ( 0.000000000000000000, 0.000000000000000000, 15.00000000000000178 ) ) ;
#3572 = AXIS2_PLACEMENT_3D ( 'NONE', #4699, #2511, #3977 ) ;
#3573 = DIRECTION ( 'NONE',  ( 1.000000000000000000, 0.000000000000000000, 0.000000000000000000 ) ) ;
#3574 = CARTESIAN_POINT ( 'NONE',  ( -5.409090909090905619, 49.00000000000000000, 8.004140804536053366 ) ) ;
#3575 = SHAPE_DEFINITION_REPRESENTATION ( #3505, #3050 ) ;
#3576 = DIRECTION ( 'NONE',  ( 0.000000000000000000, 1.000000000000000000, 0.000000000000000000 ) ) ;
#3577 = EDGE_CURVE ( 'NONE', #3515, #3799, #1263, .T. ) ;
#3578 = EDGE_CURVE ( 'NONE', #4099, #4118, #950, .T. ) ;
#3579 = FACE_BOUND ( 'NONE', #1659, .T. ) ;
#3580 = CYLINDRICAL_SURFACE ( 'NONE', #4439, 1.000000000000000000 ) ;
#3581 = DIRECTION ( 'NONE',  ( -0.000000000000000000, -1.000000000000000000, -0.000000000000000000 ) ) ;
#3582 = VECTOR ( 'NONE', #4234, 1000.000000000000000 ) ;
#3583 = APPLICATION_CONTEXT ( 'automotive_design' ) ;
#3584 = ORIENTED_EDGE ( 'NONE', *, *, #1034, .F. ) ;
#3585 = EDGE_LOOP ( 'NONE', ( #2250, #1852, #3728, #2266 ) ) ;
#3586 = VECTOR ( 'NONE', #2074, 1000.000000000000000 ) ;
#3587 = DIRECTION ( 'NONE',  ( 0.000000000000000000, 1.000000000000000000, 0.000000000000000000 ) ) ;
#3588 = SHAPE_REPRESENTATION_RELATIONSHIP ( 'NONE' , 'NONE' ,  #3050, #3930 ) ;
#3589 = SURFACE_STYLE_FILL_AREA ( #984 ) ;
#3590 = DIRECTION ( 'NONE',  ( 0.000000000000000000, 0.000000000000000000, 1.000000000000000000 ) ) ;
#3591 = ORIENTED_EDGE ( 'NONE', *, *, #1524, .F. ) ;
#3592 = FACE_OUTER_BOUND ( 'NONE', #2526, .T. ) ;
#3593 = EDGE_CURVE ( 'NONE', #3730, #3829, #2175, .T. ) ;
#3594 = CARTESIAN_POINT ( 'NONE',  ( -27.17157287525386877, 32.82842712474614899, 8.999999999999992895 ) ) ;
#3595 = EDGE_CURVE ( 'NONE', #1270, #2307, #1096, .T. ) ;
#3596 = CARTESIAN_POINT ( 'NONE',  ( 12.00000000000001954, 44.99999999999999289, 0.000000000000000000 ) ) ;
#3597 = DIRECTION ( 'NONE',  ( 0.000000000000000000, -0.000000000000000000, -1.000000000000000000 ) ) ;
#3598 = ADVANCED_FACE ( 'NONE', ( #1772 ), #3970, .T. ) ;
#3599 = SURFACE_STYLE_USAGE ( .BOTH. , #2235 ) ;
#3600 = LINE ( 'NONE', #2818, #4068 ) ;
#3601 = PRODUCT_CONTEXT ( 'NONE', #4013, 'mechanical' ) ;
#3602 = AXIS2_PLACEMENT_3D ( 'NONE', #1395, #3224, #3270 ) ;
#3603 = CIRCLE ( 'NONE', #1701, 4.000000000000000000 ) ;
#3604 = CARTESIAN_POINT ( 'NONE',  ( 0.5000000000000000000, 6.000000000000000000, 20.00000000000000000 ) ) ;
#3605 = DIRECTION ( 'NONE',  ( 0.000000000000000000, 0.000000000000000000, 1.000000000000000000 ) ) ;
#3606 = DIRECTION ( 'NONE',  ( -0.000000000000000000, -0.000000000000000000, 1.000000000000000000 ) ) ;
#3607 = CIRCLE ( 'NONE', #962, 1.750000000000001554 ) ;
#3608 = ORIENTED_EDGE ( 'NONE', *, *, #3705, .T. ) ;
#3609 = ORIENTED_EDGE ( 'NONE', *, *, #2811, .F. ) ;
#3610 = LINE ( 'NONE', #717, #1833 ) ;
#3611 = FACE_BOUND ( 'NONE', #2093, .T. ) ;
#3612 = VERTEX_POINT ( 'NONE', #2822 ) ;
#3613 = ORIENTED_EDGE ( 'NONE', *, *, #3457, .F. ) ;
#3614 = ORIENTED_EDGE ( 'NONE', *, *, #3675, .T. ) ;
#3615 = AXIS2_PLACEMENT_3D ( 'NONE', #2360, #1370, #2448 ) ;
#3616 = VECTOR ( 'NONE', #3059, 1000.000000000000000 ) ;
#3617 = DIRECTION ( 'NONE',  ( 0.000000000000000000, 0.000000000000000000, 1.000000000000000000 ) ) ;
#3618 = EDGE_CURVE ( 'NONE', #2296, #85, #324, .T. ) ;
#3619 = CARTESIAN_POINT ( 'NONE',  ( 3.464101615137757495, 33.00000000000000000, 10.99999999999999467 ) ) ;
#3620 = LINE ( 'NONE', #359, #342 ) ;
#3621 = PRESENTATION_STYLE_ASSIGNMENT (( #3599 ) ) ;
#3622 = EDGE_CURVE ( 'NONE', #4120, #4371, #1018, .T. ) ;
#3623 = ADVANCED_FACE ( 'NONE', ( #4690 ), #1459, .F. ) ;
#3624 = CARTESIAN_POINT ( 'NONE',  ( 23.83634335050103203, 18.21624151457274365, 9.526033398219871273 ) ) ;
#3625 = APPLICATION_PROTOCOL_DEFINITION ( 'draft international standard', 'automotive_design', 1998, #3836 ) ;
#3626 = CARTESIAN_POINT ( 'NONE',  ( 0.000000000000000000, 0.000000000000000000, 20.00000000000000000 ) ) ;
#3627 = CARTESIAN_POINT ( 'NONE',  ( -0.7500000000000001110, 0.000000000000000000, 18.19999999999999929 ) ) ;
#3628 = AXIS2_PLACEMENT_3D ( 'NONE', #884, #1572, #3023 ) ;
#3629 = LINE ( 'NONE', #1439, #4373 ) ;
#3630 = EDGE_LOOP ( 'NONE', ( #645, #1775, #2720, #1667 ) ) ;
#3631 = ORIENTED_EDGE ( 'NONE', *, *, #2794, .F. ) ;
#3632 = CARTESIAN_POINT ( 'NONE',  ( -3.523178763948781711, 32.34692174699498679, 7.105158153061386983 ) ) ;
#3633 = ADVANCED_FACE ( 'NONE', ( #3248 ), #1114, .T. ) ;
#3634 = DIRECTION ( 'NONE',  ( 0.000000000000000000, 0.000000000000000000, -1.000000000000000000 ) ) ;
#3635 = ORIENTED_EDGE ( 'NONE', *, *, #1453, .T. ) ;
#3636 = EDGE_CURVE ( 'NONE', #1877, #3492, #3748, .T. ) ;
#3637 =( GEOMETRIC_REPRESENTATION_CONTEXT ( 3 ) GLOBAL_UNCERTAINTY_ASSIGNED_CONTEXT ( ( #2972 ) ) GLOBAL_UNIT_ASSIGNED_CONTEXT ( ( #917, #967, #4226 ) ) REPRESENTATION_CONTEXT ( 'NONE', 'WORKASPACE' ) );
#3638 = ORIENTED_EDGE ( 'NONE', *, *, #3001, .T. ) ;
#3639 = ORIENTED_EDGE ( 'NONE', *, *, #2272, .T. ) ;
#3640 = CARTESIAN_POINT ( 'NONE',  ( 10.25000000000000178, 36.00000000000000000, 2.143131898507893689E-16 ) ) ;
#3641 = FACE_OUTER_BOUND ( 'NONE', #1492, .T. ) ;
#3642 = FACE_BOUND ( 'NONE', #549, .T. ) ;
#3643 = ORIENTED_EDGE ( 'NONE', *, *, #4405, .F. ) ;
#3644 = CARTESIAN_POINT ( 'NONE',  ( -0.7500000000000000000, 0.000000000000000000, 17.69999999999999929 ) ) ;
#3645 = CARTESIAN_POINT ( 'NONE',  ( 3.775090262067429148, 31.49720376393407761, 10.32592777499123926 ) ) ;
#3646 = PRODUCT_CONTEXT ( 'NONE', #2795, 'mechanical' ) ;
#3647 = MECHANICAL_DESIGN_GEOMETRIC_PRESENTATION_REPRESENTATION (  '', ( #2509 ), #3268 ) ;
#3648 = PRODUCT_DEFINITION ( 'UNKNOWN', '', #4612, #2809 ) ;
#3649 = CARTESIAN_POINT ( 'NONE',  ( 23.85222316637486273, 18.19536891688240843, 8.999999999999992895 ) ) ;
#3650 = DIRECTION ( 'NONE',  ( -0.000000000000000000, -0.000000000000000000, -1.000000000000000000 ) ) ;
#3651 = CARTESIAN_POINT ( 'NONE',  ( 3.959305671612554781E-15, 33.00000000000000000, 12.99999999999999289 ) ) ;
#3652 = ORIENTED_EDGE ( 'NONE', *, *, #4064, .F. ) ;
#3653 = ORIENTED_EDGE ( 'NONE', *, *, #1240, .T. ) ;
#3654 = FACE_OUTER_BOUND ( 'NONE', #3672, .T. ) ;
#3655 = AXIS2_PLACEMENT_3D ( 'NONE', #3990, #1840, #1087 ) ;
#3656 = SHAPE_REPRESENTATION_RELATIONSHIP ( 'NONE' , 'NONE' ,  #3681, #3296 ) ;
#3657 = DIRECTION ( 'NONE',  ( 0.000000000000000000, 0.000000000000000000, -1.000000000000000000 ) ) ;
#3658 = EDGE_LOOP ( 'NONE', ( #4048, #1730, #827, #1218 ) ) ;
#3659 = ORIENTED_EDGE ( 'NONE', *, *, #3041, .F. ) ;
#3660 = ORIENTED_EDGE ( 'NONE', *, *, #2429, .F. ) ;
#3661 = TOROIDAL_SURFACE ( 'NONE', #1609, 2.999999999999999112, 1.749999999999999778 ) ;
#3662 = DIRECTION ( 'NONE',  ( -0.7071067811865487940, -0.7071067811865463515, 0.000000000000000000 ) ) ;
#3663 = CARTESIAN_POINT ( 'NONE',  ( -18.36067068532948099, 23.72542776831230071, 10.29518969959635299 ) ) ;
#3664 = CARTESIAN_POINT ( 'NONE',  ( 3.469446951953614189E-15, 25.00000000000000000, 4.999999999999992006 ) ) ;
#3665 = CARTESIAN_POINT ( 'NONE',  ( 25.16843286583315020, -6.741346781237215424, 20.00001200000000168 ) ) ;
#3666 = ORIENTED_EDGE ( 'NONE', *, *, #3622, .F. ) ;
#3667 = DIRECTION ( 'NONE',  ( 1.000000000000000000, -0.000000000000000000, 0.000000000000000000 ) ) ;
#3668 = CARTESIAN_POINT ( 'NONE',  ( 23.34316218245341190, 18.84457784187173246, 6.560806493199571321 ) ) ;
#3669 = CIRCLE ( 'NONE', #409, 4.000000000000000000 ) ;
#3670 = CARTESIAN_POINT ( 'NONE',  ( -3.595210675795415867, 29.78396494222454294, 7.227341970420264161 ) ) ;
#3671 = CARTESIAN_POINT ( 'NONE',  ( -3.993226401463528141, 34.98654878845945859, 9.266623410949812012 ) ) ;
#3672 = EDGE_LOOP ( 'NONE', ( #2634, #4594, #2182, #2226 ) ) ;
#3673 = ORIENTED_EDGE ( 'NONE', *, *, #3074, .T. ) ;
#3674 = AXIS2_PLACEMENT_3D ( 'NONE', #3149, #3867, #2348 ) ;
#3675 = EDGE_CURVE ( 'NONE', #895, #2577, #2914, .T. ) ;
#3676 = CARTESIAN_POINT ( 'NONE',  ( -3.464101615137750390, 33.00000000000000000, 6.999999999999991118 ) ) ;
#3677 = CIRCLE ( 'NONE', #1261, 0.7500000000000001110 ) ;
#3678 = CARTESIAN_POINT ( 'NONE',  ( 4.528983652092195555, 49.00000000000000000, 12.12062607165318973 ) ) ;
#3679 = ORIENTED_EDGE ( 'NONE', *, *, #2306, .F. ) ;
#3680 = EDGE_LOOP ( 'NONE', ( #4041, #53, #3, #1612 ) ) ;
#3681 = SHAPE_REPRESENTATION ( 'stop button', ( #2928 ), #2543 ) ;
#3682 = VERTEX_POINT ( 'NONE', #4707 ) ;
#3683 = DIRECTION ( 'NONE',  ( -0.000000000000000000, -1.000000000000000000, 0.000000000000000000 ) ) ;
#3684 = CARTESIAN_POINT ( 'NONE',  ( -23.85222316637485562, 18.19536891688241198, 8.999999999999992895 ) ) ;
#3685 = DIRECTION ( 'NONE',  ( 0.000000000000000000, 0.000000000000000000, 1.000000000000000000 ) ) ;
#3686 = CARTESIAN_POINT ( 'NONE',  ( -26.00000000000000355, -1.701696020694477784, 20.00001200000000523 ) ) ;
#3687 = VERTEX_POINT ( 'NONE', #756 ) ;
#3688 =( GEOMETRIC_REPRESENTATION_CONTEXT ( 3 ) GLOBAL_UNCERTAINTY_ASSIGNED_CONTEXT ( ( #3732 ) ) GLOBAL_UNIT_ASSIGNED_CONTEXT ( ( #4126, #2712, #4179 ) ) REPRESENTATION_CONTEXT ( 'NONE', 'WORKASPACE' ) );
#3689 = CIRCLE ( 'NONE', #1862, 1.000000000000000888 ) ;
#3690 = PLANE ( 'NONE',  #4555 ) ;
#3691 =( GEOMETRIC_REPRESENTATION_CONTEXT ( 3 ) GLOBAL_UNCERTAINTY_ASSIGNED_CONTEXT ( ( #1574 ) ) GLOBAL_UNIT_ASSIGNED_CONTEXT ( ( #1723, #1015, #1212 ) ) REPRESENTATION_CONTEXT ( 'NONE', 'WORKASPACE' ) );
#3692 = AXIS2_PLACEMENT_3D ( 'NONE', #2900, #4354, #2876 ) ;
#3693 = DIRECTION ( 'NONE',  ( 1.000000000000000000, 0.000000000000000000, 0.000000000000000000 ) ) ;
#3694 = CARTESIAN_POINT ( 'NONE',  ( 3.959305671612555570E-15, 34.00000000000000000, 4.999999999999990230 ) ) ;
#3695 = DIRECTION ( 'NONE',  ( 1.000000000000000000, -1.621111868633889227E-15, 0.000000000000000000 ) ) ;
#3696 = DIRECTION ( 'NONE',  ( 1.000000000000000000, -8.560005772541128451E-15, 0.000000000000000000 ) ) ;
#3697 = VERTEX_POINT ( 'NONE', #1437 ) ;
#3698 = EDGE_CURVE ( 'NONE', #2996, #3949, #2891, .T. ) ;
#3699 = EDGE_LOOP ( 'NONE', ( #802, #2557 ) ) ;
#3700 = EDGE_CURVE ( 'NONE', #2552, #2995, #1064, .T. ) ;
#3701 = CARTESIAN_POINT ( 'NONE',  ( 0.000000000000000000, 0.000000000000000000, 19.00000000000000000 ) ) ;
#3702 = CIRCLE ( 'NONE', #2332, 5.500000000000000000 ) ;
#3703 = CARTESIAN_POINT ( 'NONE',  ( -4.528983652092253287, 37.00000000000000000, 12.12062607165309558 ) ) ;
#3704 = CARTESIAN_POINT ( 'NONE',  ( 0.000000000000000000, 0.000000000000000000, 19.50000000000000000 ) ) ;
#3705 = EDGE_CURVE ( 'NONE', #1315, #2385, #1752, .T. ) ;
#3706 = VERTEX_POINT ( 'NONE', #3200 ) ;
#3707 = ORIENTED_EDGE ( 'NONE', *, *, #3480, .T. ) ;
#3708 = ORIENTED_EDGE ( 'NONE', *, *, #3532, .T. ) ;
#3709 = EDGE_CURVE ( 'NONE', #2338, #1543, #2527, .T. ) ;
#3710 = TOROIDAL_SURFACE ( 'NONE', #520, 4.000000000000001776, 1.000000000000000000 ) ;
#3711 = PLANE ( 'NONE',  #144 ) ;
#3712 = DIRECTION ( 'NONE',  ( 1.000000000000000000, 0.000000000000000000, 0.000000000000000000 ) ) ;
#3713 = MECHANICAL_DESIGN_GEOMETRIC_PRESENTATION_REPRESENTATION (  '', ( #1889 ), #529 ) ;
#3714 = ORIENTED_EDGE ( 'NONE', *, *, #4060, .T. ) ;
#3715 = AXIS2_PLACEMENT_3D ( 'NONE', #3895, #1727, #619 ) ;
#3716 = CARTESIAN_POINT ( 'NONE',  ( -26.00000000000000711, 0.000000000000000000, 20.00000000000000000 ) ) ;
#3717 = DIRECTION ( 'NONE',  ( -1.000000000000000000, 0.000000000000000000, 0.000000000000000000 ) ) ;
#3718 = AXIS2_PLACEMENT_3D ( 'NONE', #1618, #649, #3206 ) ;
#3719 = CARTESIAN_POINT ( 'NONE',  ( 3.959305671612554781E-15, 37.00000000000000000, 12.99999999999999289 ) ) ;
#3720 = LINE ( 'NONE', #1920, #4362 ) ;
#3721 = CARTESIAN_POINT ( 'NONE',  ( -3.601048973789305219, 34.01100974488973350, 10.74504312029988107 ) ) ;
#3722 = AXIS2_PLACEMENT_3D ( 'NONE', #1075, #2180, #3634 ) ;
#3723 = VERTEX_POINT ( 'NONE', #389 ) ;
#3724 = ADVANCED_FACE ( 'NONE', ( #2846 ), #2477, .T. ) ;
#3725 = CARTESIAN_POINT ( 'NONE',  ( -3.810302108970980761, 31.40405275936838336, 7.767247897850001692 ) ) ;
#3726 = LINE ( 'NONE', #471, #1283 ) ;
#3727 = CARTESIAN_POINT ( 'NONE',  ( 9.000000000000003553, 36.00000000000000000, 0.000000000000000000 ) ) ;
#3728 = ORIENTED_EDGE ( 'NONE', *, *, #390, .F. ) ;
#3729 = VERTEX_POINT ( 'NONE', #2132 ) ;
#3730 = VERTEX_POINT ( 'NONE', #690 ) ;
#3731 = ORIENTED_EDGE ( 'NONE', *, *, #2586, .F. ) ;
#3732 = UNCERTAINTY_MEASURE_WITH_UNIT (LENGTH_MEASURE( 1.000000000000000082E-05 ), #4126, 'distance_accuracy_value', 'NONE');
#3733 = CARTESIAN_POINT ( 'NONE',  ( 3.469446951953614189E-15, 41.00000000000000000, 8.999999999999992895 ) ) ;
#3734 = CARTESIAN_POINT ( 'NONE',  ( -20.28376480839715157, 22.10492369241840649, 12.79609622574099070 ) ) ;
#3735 = CARTESIAN_POINT ( 'NONE',  ( 3.120626071653185285, 43.00000000000000000, 4.471016347907789346 ) ) ;
#3736 = TOROIDAL_SURFACE ( 'NONE', #3655, 12.00000000000000000, 1.749999999999999778 ) ;
#3737 = ADVANCED_FACE ( 'NONE', ( #1373 ), #3580, .F. ) ;
#3738 = ORIENTED_EDGE ( 'NONE', *, *, #3698, .T. ) ;
#3739 = APPLICATION_CONTEXT ( 'automotive_design' ) ;
#3740 = ADVANCED_FACE ( 'NONE', ( #1532 ), #2601, .F. ) ;
#3741 = EDGE_CURVE ( 'NONE', #1957, #3924, #4679, .T. ) ;
#3742 = DIRECTION ( 'NONE',  ( -0.000000000000000000, -1.000000000000000000, 0.000000000000000000 ) ) ;
#3743 = CARTESIAN_POINT ( 'NONE',  ( 3.469446951953614189E-15, 41.00000000000000000, 8.999999999999992895 ) ) ;
#3744 = AXIS2_PLACEMENT_3D ( 'NONE', #3144, #986, #3235 ) ;
#3745 = CARTESIAN_POINT ( 'NONE',  ( -1.290629128713961293, 29.97320584640673147, 5.204870533884474071 ) ) ;
#3746 = DIRECTION ( 'NONE',  ( -1.000000000000000000, 0.000000000000000000, 0.000000000000000000 ) ) ;
#3747 = ORIENTED_EDGE ( 'NONE', *, *, #3245, .F. ) ;
#3748 = CIRCLE ( 'NONE', #4221, 5.500000000000000000 ) ;
#3749 = LINE ( 'NONE', #1973, #2899 ) ;
#3750 = DIRECTION ( 'NONE',  ( 0.000000000000000000, 0.000000000000000000, 1.000000000000000000 ) ) ;
#3751 = CARTESIAN_POINT ( 'NONE',  ( 3.889087296526035242, 49.00000000000000000, 6.110912703473999841 ) ) ;
#3752 = ORIENTED_EDGE ( 'NONE', *, *, #4502, .T. ) ;
#3753 = VECTOR ( 'NONE', #3030, 1000.000000000000000 ) ;
#3754 = ORIENTED_EDGE ( 'NONE', *, *, #198, .T. ) ;
#3755 = ORIENTED_EDGE ( 'NONE', *, *, #3246, .F. ) ;
#3756 = ORIENTED_EDGE ( 'NONE', *, *, #3495, .F. ) ;
#3757 = CARTESIAN_POINT ( 'NONE',  ( -24.00000000000000355, 2.939152317953648289E-15, 17.00000000000000000 ) ) ;
#3758 =( NAMED_UNIT ( * ) PLANE_ANGLE_UNIT ( ) SI_UNIT ( $, .RADIAN. ) );
#3759=STYLED_ITEM('',(#4757),#4556);
#3760 = UNCERTAINTY_MEASURE_WITH_UNIT (LENGTH_MEASURE( 1.000000000000000082E-05 ), #4398, 'distance_accuracy_value', 'NONE');
#3761 = SURFACE_SIDE_STYLE ('',( #4598 ) ) ;
#3762 = DIRECTION ( 'NONE',  ( -0.000000000000000000, -0.000000000000000000, -1.000000000000000000 ) ) ;
#3763 = DIRECTION ( 'NONE',  ( 0.000000000000000000, 0.000000000000000000, -1.000000000000000000 ) ) ;
#3764 = AXIS2_PLACEMENT_3D ( 'NONE', #3565, #330, #673 ) ;
#3765 = EDGE_CURVE ( 'NONE', #2120, #1602, #3720, .T. ) ;
#3766 = DIRECTION ( 'NONE',  ( 0.000000000000000000, 0.000000000000000000, 1.000000000000000000 ) ) ;
#3767 = CYLINDRICAL_SURFACE ( 'NONE', #3322, 5.500000000000000000 ) ;
#3768 = DIRECTION ( 'NONE',  ( 0.000000000000000000, 0.000000000000000000, -1.000000000000000000 ) ) ;
#3769 =( GEOMETRIC_REPRESENTATION_CONTEXT ( 3 ) GLOBAL_UNCERTAINTY_ASSIGNED_CONTEXT ( ( #453 ) ) GLOBAL_UNIT_ASSIGNED_CONTEXT ( ( #1801, #1445, #4353 ) ) REPRESENTATION_CONTEXT ( 'NONE', 'WORKASPACE' ) );
#3770 = ORIENTED_EDGE ( 'NONE', *, *, #3705, .F. ) ;
#3771 = AXIS2_PLACEMENT_3D ( 'NONE', #4491, #3012, #4467 ) ;
#3772 = EDGE_CURVE ( 'NONE', #3204, #2636, #4391, .T. ) ;
#3773 = ADVANCED_FACE ( 'NONE', ( #3034 ), #93, .T. ) ;
#3774 = PRODUCT ( 'casing', 'casing', '', ( #4035 ) ) ;
#3775 =( GEOMETRIC_REPRESENTATION_CONTEXT ( 3 ) GLOBAL_UNCERTAINTY_ASSIGNED_CONTEXT ( ( #1960 ) ) GLOBAL_UNIT_ASSIGNED_CONTEXT ( ( #3300, #1144, #1511 ) ) REPRESENTATION_CONTEXT ( 'NONE', 'WORKASPACE' ) );
#3776 = VECTOR ( 'NONE', #375, 1000.000000000000000 ) ;
#3777 = DIRECTION ( 'NONE',  ( 0.000000000000000000, 0.000000000000000000, 1.000000000000000000 ) ) ;
#3778 = DIRECTION ( 'NONE',  ( -0.7071067811865484609, 0.000000000000000000, 0.7071067811865467956 ) ) ;
#3779 = B_SPLINE_CURVE_WITH_KNOTS ( 'NONE', 3,
 ( #3369, #2990, #4043, #445, #73, #4447, #47, #2898, #4351, #1463, #1487, #3996, #1163, #2179, #2630, #3298, #1186, #2946, #4397, #2267, #3725, #785, #2554, #3276, #738, #3632, #2221, #1120, #4372, #3676 ),
 .UNSPECIFIED., .F., .F.,
 ( 4, 2, 2, 2, 2, 2, 2, 2, 2, 2, 2, 2, 2, 2, 4 ),
 ( 0.006361193818781107380, 0.006758065648931978198, 0.007154937479082849015, 0.007551809309233719833, 0.007948681139384591518, 0.008345552969535447591, 0.008742424799686305398, 0.009536168459988021012, 0.009933040290138880554, 0.01032991212028973836, 0.01112365578059145224, 0.01152052761074230137, 0.01191739944089315051, 0.01231427127104400138, 0.01271114310119485051 ),
 .UNSPECIFIED. ) ;
#3780 = CARTESIAN_POINT ( 'NONE',  ( -21.02743970908340287, 21.39894891851812986, 5.000096751259999195 ) ) ;
#3781 = CARTESIAN_POINT ( 'NONE',  ( 4.000056596598889236, 35.00011319322931769, 8.869325943800760115 ) ) ;
#3782 = FACE_OUTER_BOUND ( 'NONE', #826, .T. ) ;
#3783 = ORIENTED_EDGE ( 'NONE', *, *, #1517, .T. ) ;
#3784 = ORIENTED_EDGE ( 'NONE', *, *, #132, .F. ) ;
#3785 = VERTEX_POINT ( 'NONE', #780 ) ;
#3786 = EDGE_LOOP ( 'NONE', ( #3295, #2253, #4454, #70 ) ) ;
#3787 = EDGE_CURVE ( 'NONE', #2296, #3335, #2374, .T. ) ;
#3788 = CARTESIAN_POINT ( 'NONE',  ( 3.469446951953614189E-15, 25.00000000000000000, 8.999999999999992895 ) ) ;
#3789 = FILL_AREA_STYLE_COLOUR ( '', #3880 ) ;
#3790 =( LENGTH_UNIT ( ) NAMED_UNIT ( * ) SI_UNIT ( .MILLI., .METRE. ) );
#3791 = FILL_AREA_STYLE_COLOUR ( '', #2089 ) ;
#3792 = VECTOR ( 'NONE', #3683, 1000.000000000000000 ) ;
#3793 = ORIENTED_EDGE ( 'NONE', *, *, #1999, .T. ) ;
#3794 = EDGE_CURVE ( 'NONE', #4498, #2734, #488, .T. ) ;
#3795 = DIRECTION ( 'NONE',  ( -1.000000000000000000, -0.000000000000000000, -0.000000000000000000 ) ) ;
#3796 = AXIS2_PLACEMENT_3D ( 'NONE', #306, #3926, #1013 ) ;
#3797 = FACE_OUTER_BOUND ( 'NONE', #1267, .T. ) ;
#3798 = DIRECTION ( 'NONE',  ( -1.000000000000000000, 0.000000000000000000, 0.000000000000000000 ) ) ;
#3799 = VERTEX_POINT ( 'NONE', #3011 ) ;
#3800 = AXIS2_PLACEMENT_3D ( 'NONE', #3262, #3420, #98 ) ;
#3801 = AXIS2_PLACEMENT_3D ( 'NONE', #3816, #862, #3455 ) ;
#3802 = PLANE ( 'NONE',  #260 ) ;
#3803 = CYLINDRICAL_SURFACE ( 'NONE', #3089, 0.7500000000000001110 ) ;
#3804 = EDGE_CURVE ( 'NONE', #614, #1643, #489, .T. ) ;
#3805 = ADVANCED_FACE ( 'NONE', ( #2624 ), #3394, .T. ) ;
#3806 = DIRECTION ( 'NONE',  ( 0.000000000000000000, -0.000000000000000000, 1.000000000000000000 ) ) ;
#3807 = FACE_OUTER_BOUND ( 'NONE', #1449, .T. ) ;
#3808 = DIRECTION ( 'NONE',  ( -1.000000000000000000, 0.000000000000000000, 0.000000000000000000 ) ) ;
#3809 = ORIENTED_EDGE ( 'NONE', *, *, #2599, .F. ) ;
#3810 = VECTOR ( 'NONE', #2784, 1000.000000000000000 ) ;
#3811 = EDGE_LOOP ( 'NONE', ( #4400, #2457, #3150, #623 ) ) ;
#3812 = ORIENTED_EDGE ( 'NONE', *, *, #4301, .F. ) ;
#3813 = ORIENTED_EDGE ( 'NONE', *, *, #2110, .F. ) ;
#3814 = LINE ( 'NONE', #1638, #4630 ) ;
#3815 = DIRECTION ( 'NONE',  ( 1.000000000000000000, 0.000000000000000000, 0.000000000000000000 ) ) ;
#3816 = CARTESIAN_POINT ( 'NONE',  ( 0.000000000000000000, 0.000000000000000000, 20.00000000000000000 ) ) ;
#3817 = CARTESIAN_POINT ( 'NONE',  ( 0.000000000000000000, 0.000000000000000000, 20.00000000000000000 ) ) ;
#3818 = DIRECTION ( 'NONE',  ( -1.000000000000000000, 0.000000000000000000, 0.000000000000000000 ) ) ;
#3819 = CARTESIAN_POINT ( 'NONE',  ( 3.469446951953614189E-15, 37.00000000000000000, 8.999999999999992895 ) ) ;
#3820 = CIRCLE ( 'NONE', #16, 1.000000000000000000 ) ;
#3821 = ORIENTED_EDGE ( 'NONE', *, *, #925, .F. ) ;
#3822 = AXIS2_PLACEMENT_3D ( 'NONE', #3500, #2440, #4603 ) ;
#3823 = CARTESIAN_POINT ( 'NONE',  ( -2.440392720584789288, 29.90136469312441037, 12.17998752022640296 ) ) ;
#3824 = CARTESIAN_POINT ( 'NONE',  ( 3.469446951953614189E-15, 25.00000000000000000, 8.999999999999992895 ) ) ;
#3825 = FACE_OUTER_BOUND ( 'NONE', #2020, .T. ) ;
#3826 = DIRECTION ( 'NONE',  ( -0.7071067811865487940, 0.7071067811865463515, 0.000000000000000000 ) ) ;
#3827 = CARTESIAN_POINT ( 'NONE',  ( -25.16843286583315731, 6.741346781237202102, 20.00001200000000168 ) ) ;
#3828 = ORIENTED_EDGE ( 'NONE', *, *, #3160, .T. ) ;
#3829 = VERTEX_POINT ( 'NONE', #2241 ) ;
#3830 = ORIENTED_EDGE ( 'NONE', *, *, #1129, .T. ) ;
#3831 = ADVANCED_FACE ( 'NONE', ( #4039 ), #115, .F. ) ;
#3832 = ORIENTED_EDGE ( 'NONE', *, *, #2510, .T. ) ;
#3833 = LINE ( 'NONE', #3185, #2406 ) ;
#3834 = EDGE_CURVE ( 'NONE', #1513, #956, #3988, .T. ) ;
#3835 = SURFACE_STYLE_USAGE ( .BOTH. , #2389 ) ;
#3836 = APPLICATION_CONTEXT ( 'automotive_design' ) ;
#3837 = VECTOR ( 'NONE', #347, 1000.000000000000000 ) ;
#3838 = CARTESIAN_POINT ( 'NONE',  ( 0.000000000000000000, 0.000000000000000000, 17.99999999999998579 ) ) ;
#3839 = ORIENTED_EDGE ( 'NONE', *, *, #3956, .T. ) ;
#3840 = CIRCLE ( 'NONE', #4365, 26.00000000000000355 ) ;
#3841 = CARTESIAN_POINT ( 'NONE',  ( 0.000000000000000000, 0.000000000000000000, 20.00000000000000000 ) ) ;
#3842 = DIRECTION ( 'NONE',  ( 0.000000000000000000, 0.000000000000000000, 1.000000000000000000 ) ) ;
#3843 = CARTESIAN_POINT ( 'NONE',  ( 9.000000000000003553, 36.00000000000000000, 0.000000000000000000 ) ) ;
#3844 = ORIENTED_EDGE ( 'NONE', *, *, #3188, .T. ) ;
#3845 = CYLINDRICAL_SURFACE ( 'NONE', #1432, 5.500000000000000000 ) ;
#3846 = MECHANICAL_DESIGN_GEOMETRIC_PRESENTATION_REPRESENTATION (  '', ( #2621 ), #2933 ) ;
#3847 = CARTESIAN_POINT ( 'NONE',  ( 21.02424009228912993, 21.40213195504970756, 12.99981531858142425 ) ) ;
#3848 = EDGE_CURVE ( 'NONE', #3402, #3855, #1557, .T. ) ;
#3849 = DIRECTION ( 'NONE',  ( -1.000000000000000000, 0.000000000000000000, -0.000000000000000000 ) ) ;
#3850 = AXIS2_PLACEMENT_3D ( 'NONE', #4136, #3155, #3131 ) ;
#3851 = FACE_OUTER_BOUND ( 'NONE', #3585, .T. ) ;
#3852 = DIRECTION ( 'NONE',  ( 1.000000000000000000, 0.000000000000000000, -0.000000000000000000 ) ) ;
#3853 = AXIS2_PLACEMENT_3D ( 'NONE', #166, #2016, #2292 ) ;
#3854 = CARTESIAN_POINT ( 'NONE',  ( 0.5000000000000001110, 10.00000000000000000, 15.00000000000000178 ) ) ;
#3855 = VERTEX_POINT ( 'NONE', #415 ) ;
#3856 = ORIENTED_EDGE ( 'NONE', *, *, #3207, .F. ) ;
#3857 = EDGE_CURVE ( 'NONE', #2030, #2679, #708, .T. ) ;
#3858 = ORIENTED_EDGE ( 'NONE', *, *, #3480, .F. ) ;
#3859 = CARTESIAN_POINT ( 'NONE',  ( 25.99519186311192342, -0.5000000000000000000, 19.00000000000000000 ) ) ;
#3860 = FACE_OUTER_BOUND ( 'NONE', #204, .T. ) ;
#3861 = CARTESIAN_POINT ( 'NONE',  ( 2.255140518769849223E-14, 34.17157287525380838, 3.499999999999992895 ) ) ;
#3862 = VERTEX_POINT ( 'NONE', #563 ) ;
#3863 = ADVANCED_FACE ( 'NONE', ( #182 ), #3486, .F. ) ;
#3864 = LINE ( 'NONE', #2812, #3586 ) ;
#3865 = DIRECTION ( 'NONE',  ( 1.000000000000000000, 0.000000000000000000, 0.000000000000000000 ) ) ;
#3866 = AXIS2_PLACEMENT_3D ( 'NONE', #1450, #2185, #1078 ) ;
#3867 = DIRECTION ( 'NONE',  ( -0.000000000000000000, -1.000000000000000000, -0.000000000000000000 ) ) ;
#3868 = VERTEX_POINT ( 'NONE', #922 ) ;
#3869 = AXIS2_PLACEMENT_3D ( 'NONE', #3504, #4633, #615 ) ;
#3870 = CARTESIAN_POINT ( 'NONE',  ( 21.93211642885839296, 20.47065640071369685, 12.87299606428841159 ) ) ;
#3871 = CIRCLE ( 'NONE', #4483, 4.000000000000000000 ) ;
#3872 = CARTESIAN_POINT ( 'NONE',  ( 0.5000000000000000000, -0.8660254037844387076, 19.50000000000000000 ) ) ;
#3873 = DIRECTION ( 'NONE',  ( 0.000000000000000000, -1.000000000000000000, 0.000000000000000000 ) ) ;
#3874 = CARTESIAN_POINT ( 'NONE',  ( 0.7500000000000001110, 0.000000000000000000, 15.00000000000000178 ) ) ;
#3875 = CARTESIAN_POINT ( 'NONE',  ( 4.528983652092238188, 43.00000000000000000, 5.879373928346857348 ) ) ;
#3876 = EDGE_LOOP ( 'NONE', ( #3425, #2134, #1979, #600 ) ) ;
#3877 = ORIENTED_EDGE ( 'NONE', *, *, #864, .T. ) ;
#3878 = CARTESIAN_POINT ( 'NONE',  ( -25.99519186311192342, 0.5000000000000000000, 20.00000000000000000 ) ) ;
#3879 = DIRECTION ( 'NONE',  ( 0.000000000000000000, 1.000000000000000000, 0.000000000000000000 ) ) ;
#3880 = COLOUR_RGB ( '',0.8941176470588234615, 0.8941176470588234615, 0.8941176470588234615 ) ;
#3881 = FACE_OUTER_BOUND ( 'NONE', #599, .T. ) ;
#3882 = CARTESIAN_POINT ( 'NONE',  ( 1.000000000000000000, 0.000000000000000000, 19.50000000000000000 ) ) ;
#3883 = CARTESIAN_POINT ( 'NONE',  ( 0.000000000000000000, 0.000000000000000000, 20.00000000000000000 ) ) ;
#3884 = DIRECTION ( 'NONE',  ( 0.000000000000000000, 0.000000000000000000, -1.000000000000000000 ) ) ;
#3885 = CARTESIAN_POINT ( 'NONE',  ( 3.871533456320507494, 29.74918284297944382, 10.03884696677421395 ) ) ;
#3886 = VERTEX_POINT ( 'NONE', #3892 ) ;
#3887 = ADVANCED_FACE ( 'NONE', ( #3058 ), #3802, .F. ) ;
#3888 = EDGE_CURVE ( 'NONE', #1185, #1192, #3523, .T. ) ;
#3889 = PLANE ( 'NONE',  #2262 ) ;
#3890 = AXIS2_PLACEMENT_3D ( 'NONE', #1872, #2246, #4092 ) ;
#3891 = AXIS2_PLACEMENT_3D ( 'NONE', #1503, #779, #2240 ) ;
#3892 = CARTESIAN_POINT ( 'NONE',  ( 26.49999999999999645, -0.5000000000000000000, 19.00000000000000000 ) ) ;
#3893 = CYLINDRICAL_SURFACE ( 'NONE', #4004, 0.5000000000000001110 ) ;
#3894 = DIRECTION ( 'NONE',  ( 1.000000000000000000, 0.000000000000000000, 0.000000000000000000 ) ) ;
#3895 = CARTESIAN_POINT ( 'NONE',  ( -12.00000000000000178, 44.99999999999999289, 0.000000000000000000 ) ) ;
#3896 = CARTESIAN_POINT ( 'NONE',  ( -27.10000000000000497, -0.5999999999999998668, 19.59999999999999787 ) ) ;
#3897 = ORIENTED_EDGE ( 'NONE', *, *, #198, .F. ) ;
#3898 = ORIENTED_EDGE ( 'NONE', *, *, #390, .T. ) ;
#3899 = DIRECTION ( 'NONE',  ( 0.000000000000000000, 0.000000000000000000, 1.000000000000000000 ) ) ;
#3900 = FILL_AREA_STYLE ('',( #4241 ) ) ;
#3901 = PRESENTATION_STYLE_ASSIGNMENT (( #1778 ) ) ;
#3902 = CARTESIAN_POINT ( 'NONE',  ( 3.889087296526035242, 34.17157287525380838, 5.110912703473999841 ) ) ;
#3903 = LINE ( 'NONE', #2855, #557 ) ;
#3904 = DIRECTION ( 'NONE',  ( 1.000000000000000000, 0.000000000000000000, 0.000000000000000000 ) ) ;
#3905 = VECTOR ( 'NONE', #1369, 1000.000000000000000 ) ;
#3906 = CYLINDRICAL_SURFACE ( 'NONE', #1298, 1.749999999999999778 ) ;
#3907 = PLANE ( 'NONE',  #797 ) ;
#3908 = ORIENTED_EDGE ( 'NONE', *, *, #724, .T. ) ;
#3909 = EDGE_CURVE ( 'NONE', #3785, #2044, #1628, .T. ) ;
#3910 = CIRCLE ( 'NONE', #2375, 5.500000000000000000 ) ;
#3911 = PRESENTATION_STYLE_ASSIGNMENT (( #2059 ) ) ;
#3912 = AXIS2_PLACEMENT_3D ( 'NONE', #912, #580, #1222 ) ;
#3913 = DIRECTION ( 'NONE',  ( -1.000000000000000000, 0.000000000000000000, 0.000000000000000000 ) ) ;
#3914 = EDGE_CURVE ( 'NONE', #3514, #907, #1258, .T. ) ;
#3915 = DIRECTION ( 'NONE',  ( 0.000000000000000000, 0.000000000000000000, 1.000000000000000000 ) ) ;
#3916 = CARTESIAN_POINT ( 'NONE',  ( 20.67279826512042362, -15.85973458909328571, 20.00001200000000523 ) ) ;
#3917 = EDGE_CURVE ( 'NONE', #3361, #1928, #871, .T. ) ;
#3918 = CARTESIAN_POINT ( 'NONE',  ( 3.469446951953614189E-15, 39.99999999999999289, 8.999999999999992895 ) ) ;
#3919 = DIRECTION ( 'NONE',  ( 0.000000000000000000, 0.000000000000000000, 1.000000000000000000 ) ) ;
#3920 = DIRECTION ( 'NONE',  ( -0.000000000000000000, -1.000000000000000000, -0.000000000000000000 ) ) ;
#3921 = STYLED_ITEM ( 'NONE', ( #4504 ), #1203 ) ;
#3922 = CIRCLE ( 'NONE', #3009, 4.000000000000000000 ) ;
#3923 = APPLICATION_CONTEXT ( 'automotive_design' ) ;
#3924 = VERTEX_POINT ( 'NONE', #2864 ) ;
#3925 = VERTEX_POINT ( 'NONE', #299 ) ;
#3926 = DIRECTION ( 'NONE',  ( -0.000000000000000000, 1.000000000000000000, -0.000000000000000000 ) ) ;
#3927 = AXIS2_PLACEMENT_3D ( 'NONE', #1565, #3915, #3087 ) ;
#3928 = DIRECTION ( 'NONE',  ( -1.000000000000000000, 0.000000000000000000, 0.000000000000000000 ) ) ;
#3929 = VECTOR ( 'NONE', #2105, 1000.000000000000000 ) ;
#3930 = ADVANCED_BREP_SHAPE_REPRESENTATION ( '', ( #2889, #2928 ), #1184 ) ;
#3931 = DIRECTION ( 'NONE',  ( 0.000000000000000000, 0.000000000000000000, 1.000000000000000000 ) ) ;
#3932 = DIRECTION ( 'NONE',  ( 0.000000000000000000, 1.000000000000000000, 0.000000000000000000 ) ) ;
#3933 = EDGE_LOOP ( 'NONE', ( #550, #4395 ) ) ;
#3934 = DIRECTION ( 'NONE',  ( 0.000000000000000000, 0.000000000000000000, 1.000000000000000000 ) ) ;
#3935 = CARTESIAN_POINT ( 'NONE',  ( -26.50000000000000355, -0.5000000000000000000, 19.00000000000000000 ) ) ;
#3936 = DIRECTION ( 'NONE',  ( 0.000000000000000000, 1.000000000000000000, 0.000000000000000000 ) ) ;
#3937 = FACE_OUTER_BOUND ( 'NONE', #2245, .T. ) ;
#3938 = ADVANCED_FACE ( 'NONE', ( #1414, #2547 ), #2447, .T. ) ;
#3939 = EDGE_CURVE ( 'NONE', #4187, #3116, #647, .T. ) ;
#3940 = FACE_OUTER_BOUND ( 'NONE', #1299, .T. ) ;
#3941 = AXIS2_PLACEMENT_3D ( 'NONE', #2358, #1705, #4616 ) ;
#3942 = CARTESIAN_POINT ( 'NONE',  ( 3.501309621998943467, 32.47496340993090058, 7.065645527993491548 ) ) ;
#3943 = CARTESIAN_POINT ( 'NONE',  ( 0.9958591954639605115, 37.00000000000000000, 3.590909090909087276 ) ) ;
#3944 = CIRCLE ( 'NONE', #2327, 0.7500000000000001110 ) ;
#3945 = CARTESIAN_POINT ( 'NONE',  ( -23.23798364781088210, 18.97448886297816273, 6.357861838490105555 ) ) ;
#3946 = VECTOR ( 'NONE', #4608, 1000.000000000000000 ) ;
#3947 = DIRECTION ( 'NONE',  ( 0.000000000000000000, 0.000000000000000000, -1.000000000000000000 ) ) ;
#3948 = DIRECTION ( 'NONE',  ( -1.000000000000000000, 0.000000000000000000, 0.000000000000000000 ) ) ;
#3949 = VERTEX_POINT ( 'NONE', #1039 ) ;
#3950 = EDGE_CURVE ( 'NONE', #788, #477, #2472, .T. ) ;
#3951 = ORIENTED_EDGE ( 'NONE', *, *, #916, .T. ) ;
#3952 = CIRCLE ( 'NONE', #1505, 5.500000000000000000 ) ;
#3953 =( NAMED_UNIT ( * ) SI_UNIT ( $, .STERADIAN. ) SOLID_ANGLE_UNIT ( ) );
#3954 =( LENGTH_UNIT ( ) NAMED_UNIT ( * ) SI_UNIT ( .MILLI., .METRE. ) );
#3955 = VECTOR ( 'NONE', #1668, 1000.000000000000000 ) ;
#3956 = EDGE_CURVE ( 'NONE', #4460, #2036, #650, .T. ) ;
#3957 = DIRECTION ( 'NONE',  ( 1.000000000000000000, 0.000000000000000000, 0.000000000000000000 ) ) ;
#3958 = CYLINDRICAL_SURFACE ( 'NONE', #3961, 0.7500000000000001110 ) ;
#3959 = ORIENTED_EDGE ( 'NONE', *, *, #2983, .T. ) ;
#3960 = CARTESIAN_POINT ( 'NONE',  ( 26.00000000000000355, 1.592040838891558898E-15, 20.00000599999999906 ) ) ;
#3961 = AXIS2_PLACEMENT_3D ( 'NONE', #3999, #699, #2138 ) ;
#3962 = DIRECTION ( 'NONE',  ( 0.000000000000000000, 0.000000000000000000, 1.000000000000000000 ) ) ;
#3963 = DIRECTION ( 'NONE',  ( 0.000000000000000000, 1.000000000000000000, 0.000000000000000000 ) ) ;
#3964 = CARTESIAN_POINT ( 'NONE',  ( 3.011018170818868800, 29.84908880846061408, 11.64607938208749971 ) ) ;
#3965 = AXIS2_PLACEMENT_3D ( 'NONE', #448, #1540, #2993 ) ;
#3966 = DIRECTION ( 'NONE',  ( -0.000000000000000000, 1.000000000000000000, -0.000000000000000000 ) ) ;
#3967 = CARTESIAN_POINT ( 'NONE',  ( 0.000000000000000000, 0.000000000000000000, 19.59999999999999787 ) ) ;
#3968 = CARTESIAN_POINT ( 'NONE',  ( 0.000000000000000000, 0.000000000000000000, 0.000000000000000000 ) ) ;
#3969 = DIRECTION ( 'NONE',  ( -0.7071067811865456854, 0.000000000000000000, -0.7071067811865493491 ) ) ;
#3970 = CYLINDRICAL_SURFACE ( 'NONE', #4062, 1.749999999999999778 ) ;
#3971 = CARTESIAN_POINT ( 'NONE',  ( 3.959305671612554781E-15, 25.00000000000000000, 12.99999999999999289 ) ) ;
#3972 = CONICAL_SURFACE ( 'NONE', #2514, 5.000000000000000888, 0.7853981633974517207 ) ;
#3973 = ORIENTED_EDGE ( 'NONE', *, *, #863, .T. ) ;
#3974 = ORIENTED_EDGE ( 'NONE', *, *, #2773, .T. ) ;
#3975 = CYLINDRICAL_SURFACE ( 'NONE', #843, 26.00000000000000355 ) ;
#3976 = CIRCLE ( 'NONE', #861, 1.000000000000000000 ) ;
#3977 = DIRECTION ( 'NONE',  ( 1.000000000000000000, 0.000000000000000000, -0.000000000000000000 ) ) ;
#3978 = EDGE_CURVE ( 'NONE', #3949, #2553, #3174, .T. ) ;
#3979 = ORIENTED_EDGE ( 'NONE', *, *, #4098, .F. ) ;
#3980 = CARTESIAN_POINT ( 'NONE',  ( 11.52193136556786257, 23.36965697125208052, 20.00001200000000168 ) ) ;
#3981 = EDGE_CURVE ( 'NONE', #2022, #3258, #3600, .T. ) ;
#3982 = CARTESIAN_POINT ( 'NONE',  ( 0.000000000000000000, 0.000000000000000000, 15.00000000000000178 ) ) ;
#3983 = CARTESIAN_POINT ( 'NONE',  ( 3.672180636677260246, 34.22280265294261170, 7.412133430177196836 ) ) ;
#3984 = DIRECTION ( 'NONE',  ( 0.000000000000000000, 0.000000000000000000, 1.000000000000000000 ) ) ;
#3985 = FILL_AREA_STYLE_COLOUR ( '', #3007 ) ;
#3986 = CARTESIAN_POINT ( 'NONE',  ( 22.86660962422647358, 19.42075468095221424, 12.18297904795690378 ) ) ;
#3987 = ITEM_DEFINED_TRANSFORMATION ( 'NONE', 'NONE', #1866,  #2928 ) ;
#3988 = CIRCLE ( 'NONE', #4599, 8.000000000000000000 ) ;
#3989 = CIRCLE ( 'NONE', #4602, 1.749999999999999778 ) ;
#3990 = CARTESIAN_POINT ( 'NONE',  ( -1.734723475976807094E-15, 45.00000000000000000, 0.000000000000000000 ) ) ;
#3991 = ADVANCED_FACE ( 'NONE', ( #709, #2172 ), #2840, .F. ) ;
#3992 = DIRECTION ( 'NONE',  ( 0.000000000000000000, 0.000000000000000000, 1.000000000000000000 ) ) ;
#3993 = CARTESIAN_POINT ( 'NONE',  ( -3.471963499745391868, 33.26650496313073546, 7.013453814050720325 ) ) ;
#3994 = EDGE_LOOP ( 'NONE', ( #1568, #4452, #3067, #2803 ) ) ;
#3995 = VERTEX_POINT ( 'NONE', #3574 ) ;
#3996 = CARTESIAN_POINT ( 'NONE',  ( -3.872084230669213145, 31.26872969142421255, 10.00969786038576714 ) ) ;
#3997 = FILL_AREA_STYLE_COLOUR ( '', #2096 ) ;
#3998 = AXIS2_PLACEMENT_3D ( 'NONE', #2942, #1506, #3746 ) ;
#3999 = CARTESIAN_POINT ( 'NONE',  ( 0.000000000000000000, 20.00000000000000000, 17.69999999999999929 ) ) ;
#4000 = ORIENTED_EDGE ( 'NONE', *, *, #2537, .F. ) ;
#4001 = ORIENTED_EDGE ( 'NONE', *, *, #1916, .F. ) ;
#4002 = EDGE_LOOP ( 'NONE', ( #4172, #1685, #958, #1982, #2274, #2224 ) ) ;
#4003 = PRODUCT_DEFINITION_FORMATION_WITH_SPECIFIED_SOURCE ( 'ANY', '', #1229, .NOT_KNOWN. ) ;
#4004 = AXIS2_PLACEMENT_3D ( 'NONE', #4054, #406, #59 ) ;
#4005 = DIRECTION ( 'NONE',  ( -1.000000000000000000, 0.000000000000000000, 0.000000000000000000 ) ) ;
#4006 = CARTESIAN_POINT ( 'NONE',  ( 0.5000000000000000000, -0.8660254037844387076, 20.00000000000000000 ) ) ;
#4007 = FILL_AREA_STYLE_COLOUR ( '', #1030 ) ;
#4008 = PRODUCT_RELATED_PRODUCT_CATEGORY ( 'part', '', ( #2031 ) ) ;
#4009 = ORIENTED_EDGE ( 'NONE', *, *, #1156, .T. ) ;
#4010 = CARTESIAN_POINT ( 'NONE',  ( 3.469446951953614189E-15, 41.00000000000000000, 8.999999999999992895 ) ) ;
#4011 = CARTESIAN_POINT ( 'NONE',  ( 3.469446951953614189E-15, 49.00000000000000000, 8.999999999999992895 ) ) ;
#4012 = CONTEXT_DEPENDENT_SHAPE_REPRESENTATION ( #3010, #4459 ) ;
#4013 = APPLICATION_CONTEXT ( 'automotive_design' ) ;
#4014 = CARTESIAN_POINT ( 'NONE',  ( 23.72646225117223295, 18.35933649373362897, 7.709376215153276313 ) ) ;
#4015 = DIRECTION ( 'NONE',  ( 0.000000000000000000, 0.000000000000000000, 1.000000000000000000 ) ) ;
#4016 = AXIS2_PLACEMENT_3D ( 'NONE', #2001, #2735, #1023 ) ;
#4017 = CARTESIAN_POINT ( 'NONE',  ( -3.120626071653209266, 49.00000000000000000, 13.52898365209217246 ) ) ;
#4018 = ORIENTED_EDGE ( 'NONE', *, *, #3160, .F. ) ;
#4019 = EDGE_LOOP ( 'NONE', ( #2997, #4541, #2979, #2258, #1536, #4544 ) ) ;
#4020 = COLOUR_RGB ( '',0.8941176470588234615, 0.8941176470588234615, 0.8941176470588234615 ) ;
#4021 = DIRECTION ( 'NONE',  ( -0.7071067811865487940, 0.7071067811865463515, 0.000000000000000000 ) ) ;
#4022 = PRESENTATION_STYLE_ASSIGNMENT (( #4449 ) ) ;
#4023 = CARTESIAN_POINT ( 'NONE',  ( 0.000000000000000000, 0.000000000000000000, 19.59999999999999787 ) ) ;
#4024 = EDGE_LOOP ( 'NONE', ( #3430, #4377 ) ) ;
#4025 = ORIENTED_EDGE ( 'NONE', *, *, #1869, .F. ) ;
#4026 = AXIS2_PLACEMENT_3D ( 'NONE', #1333, #903, #2701 ) ;
#4027 = ORIENTED_EDGE ( 'NONE', *, *, #1548, .T. ) ;
#4028 = DIRECTION ( 'NONE',  ( 0.000000000000000000, 0.000000000000000000, 1.000000000000000000 ) ) ;
#4029 = CARTESIAN_POINT ( 'NONE',  ( -19.92389804225928529, 22.42982507849018958, 12.59566700906149173 ) ) ;
#4030 = CARTESIAN_POINT ( 'NONE',  ( 0.000000000000000000, 0.000000000000000000, 20.00000000000000000 ) ) ;
#4031 = CARTESIAN_POINT ( 'NONE',  ( 6.741346781237209207, -25.16843286583315731, 20.00001199999999812 ) ) ;
#4032 = EDGE_LOOP ( 'NONE', ( #44, #354, #217, #350 ) ) ;
#4033 = CARTESIAN_POINT ( 'NONE',  ( -30.00000000000000355, 0.000000000000000000, 0.000000000000000000 ) ) ;
#4034 = FACE_OUTER_BOUND ( 'NONE', #1219, .T. ) ;
#4035 = PRODUCT_CONTEXT ( 'NONE', #4178, 'mechanical' ) ;
#4036 = VECTOR ( 'NONE', #911, 1000.000000000000000 ) ;
#4037 = EDGE_CURVE ( 'NONE', #574, #1199, #939, .T. ) ;
#4038 = CARTESIAN_POINT ( 'NONE',  ( -0.7500000000000001110, 1.299038105676658450, 17.69999999999999929 ) ) ;
#4039 = FACE_OUTER_BOUND ( 'NONE', #169, .T. ) ;
#4040 = CARTESIAN_POINT ( 'NONE',  ( -0.7500000000000001110, 20.00000000000000000, 17.69999999999999929 ) ) ;
#4041 = ORIENTED_EDGE ( 'NONE', *, *, #2781, .F. ) ;
#4042 = ORIENTED_EDGE ( 'NONE', *, *, #3392, .T. ) ;
#4043 = CARTESIAN_POINT ( 'NONE',  ( -3.472015849686731048, 32.73269672721935564, 10.98645679572690170 ) ) ;
#4044 = CLOSED_SHELL ( 'NONE', ( #2958, #1702, #2168, #2192, #3773, #603, #2480, #3299, #4446, #2939, #1181, #807, #1275, #312 ) ) ;
#4045 = AXIS2_PLACEMENT_3D ( 'NONE', #278, #3554, #1394 ) ;
#4046 = FACE_OUTER_BOUND ( 'NONE', #4499, .T. ) ;
#4047 = EDGE_LOOP ( 'NONE', ( #4349, #3444, #4542, #2067 ) ) ;
#4048 = ORIENTED_EDGE ( 'NONE', *, *, #863, .F. ) ;
#4049 = ORIENTED_EDGE ( 'NONE', *, *, #230, .T. ) ;
#4050 = VECTOR ( 'NONE', #944, 1000.000000000000000 ) ;
#4051 = CARTESIAN_POINT ( 'NONE',  ( 8.999999999999984013, 32.99999999999999289, 1.749999999999999778 ) ) ;
#4052 = DIRECTION ( 'NONE',  ( -1.621111868633889227E-15, -1.000000000000000000, 0.000000000000000000 ) ) ;
#4053 = CARTESIAN_POINT ( 'NONE',  ( -25.99519186311192342, -0.5000000000000000000, 19.00000000000000000 ) ) ;
#4054 = CARTESIAN_POINT ( 'NONE',  ( 0.000000000000000000, 10.00000000000000000, 13.00000000000000178 ) ) ;
#4055 = ORIENTED_EDGE ( 'NONE', *, *, #3636, .F. ) ;
#4056 = FACE_OUTER_BOUND ( 'NONE', #1660, .T. ) ;
#4057 = DIRECTION ( 'NONE',  ( 0.000000000000000000, 0.000000000000000000, 1.000000000000000000 ) ) ;
#4058 = EDGE_CURVE ( 'NONE', #3335, #2296, #3603, .T. ) ;
#4059 = EDGE_CURVE ( 'NONE', #2849, #765, #3153, .T. ) ;
#4060 = EDGE_CURVE ( 'NONE', #1922, #1485, #2920, .T. ) ;
#4061 = CARTESIAN_POINT ( 'NONE',  ( 22.87032942663243773, 19.41638709359441606, 5.821272343678753458 ) ) ;
#4062 = AXIS2_PLACEMENT_3D ( 'NONE', #2454, #4281, #3605 ) ;
#4063 = DIRECTION ( 'NONE',  ( -1.000000000000000000, 0.000000000000000000, 0.000000000000000000 ) ) ;
#4064 = EDGE_CURVE ( 'NONE', #305, #4187, #3840, .T. ) ;
#4065 = CARTESIAN_POINT ( 'NONE',  ( -5.377642775528101993E-14, 37.00000000000000000, 14.49999999999999289 ) ) ;
#4066 = ORIENTED_EDGE ( 'NONE', *, *, #516, .F. ) ;
#4067 = ORIENTED_EDGE ( 'NONE', *, *, #2352, .T. ) ;
#4068 = VECTOR ( 'NONE', #4276, 1000.000000000000000 ) ;
#4069 = FACE_OUTER_BOUND ( 'NONE', #2316, .T. ) ;
#4070 =( GEOMETRIC_REPRESENTATION_CONTEXT ( 3 ) GLOBAL_UNCERTAINTY_ASSIGNED_CONTEXT ( ( #2254 ) ) GLOBAL_UNIT_ASSIGNED_CONTEXT ( ( #1642, #2663, #555 ) ) REPRESENTATION_CONTEXT ( 'NONE', 'WORKASPACE' ) );
#4071 = FACE_OUTER_BOUND ( 'NONE', #1569, .T. ) ;
#4072 = ORIENTED_EDGE ( 'NONE', *, *, #189, .F. ) ;
#4073 = ORIENTED_EDGE ( 'NONE', *, *, #1703, .T. ) ;
#4074 = EDGE_LOOP ( 'NONE', ( #1755, #1542 ) ) ;
#4075 = UNCERTAINTY_MEASURE_WITH_UNIT (LENGTH_MEASURE( 1.000000000000000082E-05 ), #32, 'distance_accuracy_value', 'NONE');
#4076 = CARTESIAN_POINT ( 'NONE',  ( -8.999999999999973355, 32.99999999999999289, 0.000000000000000000 ) ) ;
#4077 = CARTESIAN_POINT ( 'NONE',  ( -18.21624151457282537, 23.83634335050096809, 9.526033398219878379 ) ) ;
#4078 = LINE ( 'NONE', #108, #2308 ) ;
#4079 = DIRECTION ( 'NONE',  ( 1.000000000000000000, 0.000000000000000000, -0.000000000000000000 ) ) ;
#4080 = ORIENTED_EDGE ( 'NONE', *, *, #3622, .T. ) ;
#4081 = AXIS2_PLACEMENT_3D ( 'NONE', #3417, #3464, #3778 ) ;
#4082 =( REPRESENTATION_RELATIONSHIP ('NONE','NONE', #2397, #3681 ) REPRESENTATION_RELATIONSHIP_WITH_TRANSFORMATION ( #3031 )SHAPE_REPRESENTATION_RELATIONSHIP( ) );
#4083 = DIRECTION ( 'NONE',  ( 0.000000000000000000, 0.000000000000000000, 1.000000000000000000 ) ) ;
#4084 = PRESENTATION_LAYER_ASSIGNMENT (  '', '', ( #4696 ) ) ;
#4085 = CARTESIAN_POINT ( 'NONE',  ( -0.7500000000000001110, 0.000000000000000000, 17.69999999999999929 ) ) ;
#4086 = EDGE_CURVE ( 'NONE', #3949, #3182, #1939, .T. ) ;
#4087 = CARTESIAN_POINT ( 'NONE',  ( 18.19536891688250435, 23.85222316637480944, 8.738792385868094925 ) ) ;
#4088 = DIRECTION ( 'NONE',  ( -0.000000000000000000, 1.000000000000000000, -0.000000000000000000 ) ) ;
#4089 = CARTESIAN_POINT ( 'NONE',  ( -3.809422024637061810, 34.58617949464730401, 10.22508852591142059 ) ) ;
#4090 = VERTEX_POINT ( 'NONE', #1861 ) ;
#4091 = ORIENTED_EDGE ( 'NONE', *, *, #2475, .F. ) ;
#4092 = DIRECTION ( 'NONE',  ( -1.000000000000000000, 0.000000000000000000, -0.000000000000000000 ) ) ;
#4093 = AXIS2_PLACEMENT_3D ( 'NONE', #338, #2813, #3865 ) ;
#4094 = CARTESIAN_POINT ( 'NONE',  ( 3.472185852622990065, 33.26949845712274367, 7.013837769849709858 ) ) ;
#4095 = ADVANCED_FACE ( 'NONE', ( #4414 ), #436, .F. ) ;
#4096 = DIRECTION ( 'NONE',  ( -0.000000000000000000, -1.000000000000000000, 0.000000000000000000 ) ) ;
#4097 = EDGE_LOOP ( 'NONE', ( #1314, #561 ) ) ;
#4098 = EDGE_CURVE ( 'NONE', #213, #460, #3289, .T. ) ;
#4099 = VERTEX_POINT ( 'NONE', #775 ) ;
#4100 = VERTEX_POINT ( 'NONE', #1226 ) ;
#4101 = ORIENTED_EDGE ( 'NONE', *, *, #1177, .F. ) ;
#4102 = VECTOR ( 'NONE', #1808, 1000.000000000000000 ) ;
#4103 = DIRECTION ( 'NONE',  ( 0.000000000000000000, 0.000000000000000000, -1.000000000000000000 ) ) ;
#4104 = DIRECTION ( 'NONE',  ( 8.921435019309286191E-15, 1.000000000000000000, 0.000000000000000000 ) ) ;
#4105 = EDGE_CURVE ( 'NONE', #2482, #2135, #3527, .T. ) ;
#4106 = AXIS2_PLACEMENT_3D ( 'NONE', #1340, #936, #2366 ) ;
#4107 = CYLINDRICAL_SURFACE ( 'NONE', #2164, 30.00000000000000355 ) ;
#4108 = VERTEX_POINT ( 'NONE', #3338 ) ;
#4109 = CARTESIAN_POINT ( 'NONE',  ( 3.469446951953614189E-15, 34.00000000000000000, 8.999999999999992895 ) ) ;
#4110 = DIRECTION ( 'NONE',  ( 0.000000000000000000, 0.000000000000000000, -1.000000000000000000 ) ) ;
#4111 = PRESENTATION_LAYER_ASSIGNMENT (  '', '', ( #2509 ) ) ;
#4112 = CARTESIAN_POINT ( 'NONE',  ( 0.000000000000000000, 0.000000000000000000, 17.00000000000000000 ) ) ;
#4113 = LINE ( 'NONE', #141, #589 ) ;
#4114 = ORIENTED_EDGE ( 'NONE', *, *, #4427, .F. ) ;
#4115 = CARTESIAN_POINT ( 'NONE',  ( 0.000000000000000000, 0.000000000000000000, 20.00000000000000000 ) ) ;
#4116 = DIRECTION ( 'NONE',  ( 0.000000000000000000, 0.000000000000000000, 1.000000000000000000 ) ) ;
#4117 = DIRECTION ( 'NONE',  ( 0.000000000000000000, 0.000000000000000000, 1.000000000000000000 ) ) ;
#4118 = VERTEX_POINT ( 'NONE', #2937 ) ;
#4119 = EDGE_CURVE ( 'NONE', #468, #460, #2010, .T. ) ;
#4120 = VERTEX_POINT ( 'NONE', #4085 ) ;
#4121 = EDGE_LOOP ( 'NONE', ( #3784, #1398, #3643, #935 ) ) ;
#4122 = ORIENTED_EDGE ( 'NONE', *, *, #54, .T. ) ;
#4123 = AXIS2_PLACEMENT_3D ( 'NONE', #1562, #4470, #1209 ) ;
#4124 = DIRECTION ( 'NONE',  ( 1.000000000000000000, 0.000000000000000000, 0.000000000000000000 ) ) ;
#4125 = CARTESIAN_POINT ( 'NONE',  ( -21.02820489033399554, 21.39823644064415120, 13.00018275065233020 ) ) ;
#4126 =( LENGTH_UNIT ( ) NAMED_UNIT ( * ) SI_UNIT ( .MILLI., .METRE. ) );
#4127 = ADVANCED_FACE ( 'NONE', ( #88 ), #1472, .T. ) ;
#4128 = EDGE_CURVE ( 'NONE', #4522, #2577, #2571, .T. ) ;
#4129 = CIRCLE ( 'NONE', #4275, 1.749999999999999778 ) ;
#4130 = CARTESIAN_POINT ( 'NONE',  ( -10.25000000000000178, 36.00000000000001421, 2.143131898507868051E-16 ) ) ;
#4131 = DIRECTION ( 'NONE',  ( 0.000000000000000000, 0.000000000000000000, 1.000000000000000000 ) ) ;
#4132 = DIRECTION ( 'NONE',  ( 0.000000000000000000, 1.000000000000000000, 0.000000000000000000 ) ) ;
#4133 = FACE_BOUND ( 'NONE', #3699, .T. ) ;
#4134 = VERTEX_POINT ( 'NONE', #1528 ) ;
#4135 = DIRECTION ( 'NONE',  ( 1.000000000000000000, 0.000000000000000000, 0.000000000000000000 ) ) ;
#4136 = CARTESIAN_POINT ( 'NONE',  ( 0.000000000000000000, 0.000000000000000000, 15.00000000000000178 ) ) ;
#4137 = EDGE_CURVE ( 'NONE', #3310, #1737, #2982, .T. ) ;
#4138 = AXIS2_PLACEMENT_3D ( 'NONE', #666, #3555, #3919 ) ;
#4139 = CARTESIAN_POINT ( 'NONE',  ( -19.74853269256677990, 22.58414294016069945, 5.528858171306252345 ) ) ;
#4140 = CARTESIAN_POINT ( 'NONE',  ( 3.775946040281031646, 34.50493851269693124, 10.32350191120197813 ) ) ;
#4141 = CARTESIAN_POINT ( 'NONE',  ( 4.528983652092195555, 43.00000000000000000, 12.12062607165318973 ) ) ;
#4142 = ORIENTED_EDGE ( 'NONE', *, *, #3217, .F. ) ;
#4143 = VECTOR ( 'NONE', #818, 1000.000000000000000 ) ;
#4144 = ORIENTED_EDGE ( 'NONE', *, *, #3978, .F. ) ;
#4145 = ORIENTED_EDGE ( 'NONE', *, *, #3392, .F. ) ;
#4146 = ORIENTED_EDGE ( 'NONE', *, *, #1264, .T. ) ;
#4147 = CARTESIAN_POINT ( 'NONE',  ( -0.5000000000000000000, 6.000000000000000000, 20.00000000000000000 ) ) ;
#4148 = LINE ( 'NONE', #602, #539 ) ;
#4149 = VECTOR ( 'NONE', #888, 1000.000000000000000 ) ;
#4150 = UNCERTAINTY_MEASURE_WITH_UNIT (LENGTH_MEASURE( 1.000000000000000082E-05 ), #263, 'distance_accuracy_value', 'NONE');
#4151 = SHAPE_REPRESENTATION_RELATIONSHIP ( 'NONE' , 'NONE' ,  #773, #1203 ) ;
#4152 = CARTESIAN_POINT ( 'NONE',  ( 26.49999999999999645, 0.5000000000000000000, 19.00000000000000000 ) ) ;
#4153 = FACE_OUTER_BOUND ( 'NONE', #1447, .T. ) ;
#4154 = PRESENTATION_LAYER_ASSIGNMENT (  '', '', ( #878 ) ) ;
#4155 = DIRECTION ( 'NONE',  ( -0.000000000000000000, -0.000000000000000000, 1.000000000000000000 ) ) ;
#4156 = DIRECTION ( 'NONE',  ( 0.000000000000000000, 0.000000000000000000, 1.000000000000000000 ) ) ;
#4157 = DIRECTION ( 'NONE',  ( -1.000000000000000000, 0.000000000000000000, 0.000000000000000000 ) ) ;
#4158 = PRODUCT_RELATED_PRODUCT_CATEGORY ( 'part', '', ( #3774 ) ) ;
#4159 = STYLED_ITEM ( 'NONE', ( #1003 ), #3930 ) ;
#4160 = EDGE_LOOP ( 'NONE', ( #1214, #3375, #4476, #811, #3094, #2009, #2593, #2611 ) ) ;
#4161 = VECTOR ( 'NONE', #1533, 1000.000000000000000 ) ;
#4162 = ADVANCED_FACE ( 'NONE', ( #4034 ), #2212, .T. ) ;
#4163 = PRODUCT_DEFINITION_SHAPE ( 'NONE', 'NONE',  #4710 ) ;
#4164 = CIRCLE ( 'NONE', #3722, 0.9999999999999991118 ) ;
#4165 = CARTESIAN_POINT ( 'NONE',  ( -3.871674220476135631, 29.74916513505594295, 7.961019890438434388 ) ) ;
#4166 = DIRECTION ( 'NONE',  ( 1.000000000000000000, 0.000000000000000000, 0.000000000000000000 ) ) ;
#4167 = CARTESIAN_POINT ( 'NONE',  ( -20.84134157445931734, 21.58020450303982329, 5.025533726064749906 ) ) ;
#4168 = DIRECTION ( 'NONE',  ( -0.000000000000000000, -0.000000000000000000, -1.000000000000000000 ) ) ;
#4169 = DIRECTION ( 'NONE',  ( 0.6918751026959644168, 0.6918751026959668593, 0.2064405108957393098 ) ) ;
#4170 = CARTESIAN_POINT ( 'NONE',  ( -15.85973458909327860, 20.67279826512041652, 20.00001200000000168 ) ) ;
#4171 = ORIENTED_EDGE ( 'NONE', *, *, #3146, .F. ) ;
#4172 = ORIENTED_EDGE ( 'NONE', *, *, #579, .F. ) ;
#4173 = ORIENTED_EDGE ( 'NONE', *, *, #3917, .F. ) ;
#4174 = EDGE_LOOP ( 'NONE', ( #4025, #333, #784, #1241 ) ) ;
#4175 = AXIS2_PLACEMENT_3D ( 'NONE', #4680, #654, #4295 ) ;
#4176 = DIRECTION ( 'NONE',  ( -1.000000000000000000, 0.000000000000000000, 0.000000000000000000 ) ) ;
#4177 = CARTESIAN_POINT ( 'NONE',  ( 0.7500000000000001110, 20.00000000000000000, 18.19999999999999929 ) ) ;
#4178 = APPLICATION_CONTEXT ( 'automotive_design' ) ;
#4179 =( NAMED_UNIT ( * ) SI_UNIT ( $, .STERADIAN. ) SOLID_ANGLE_UNIT ( ) );
#4180 = CARTESIAN_POINT ( 'NONE',  ( 1.500000000000000222, 0.000000000000000000, 17.69999999999999929 ) ) ;
#4181 = AXIS2_PLACEMENT_3D ( 'NONE', #30, #2561, #2858 ) ;
#4182 = CARTESIAN_POINT ( 'NONE',  ( 3.469446951953614189E-15, 49.00000000000000000, 8.999999999999992895 ) ) ;
#4183 = CARTESIAN_POINT ( 'NONE',  ( 0.000000000000000000, 0.000000000000000000, 19.50000000000000000 ) ) ;
#4184 = AXIS2_PLACEMENT_3D ( 'NONE', #2544, #341, #2980 ) ;
#4185 = PLANE ( 'NONE',  #368 ) ;
#4186 = CARTESIAN_POINT ( 'NONE',  ( 0.000000000000000000, 0.000000000000000000, 17.00000000000000000 ) ) ;
#4187 = VERTEX_POINT ( 'NONE', #111 ) ;
#4188 = AXIS2_PLACEMENT_3D ( 'NONE', #2464, #4627, #1738 ) ;
#4189 = CARTESIAN_POINT ( 'NONE',  ( -13.75000000000000000, 36.00000000000001421, 0.000000000000000000 ) ) ;
#4190 = EDGE_CURVE ( 'NONE', #22, #2966, #39, .T. ) ;
#4191 = LINE ( 'NONE', #517, #2778 ) ;
#4192 = ADVANCED_FACE ( 'NONE', ( #4558 ), #1940, .T. ) ;
#4193 = DIRECTION ( 'NONE',  ( -1.927470528863123239E-16, 1.000000000000000000, 0.000000000000000000 ) ) ;
#4194 = DIRECTION ( 'NONE',  ( 0.000000000000000000, 0.000000000000000000, 1.000000000000000000 ) ) ;
#4195 = DIRECTION ( 'NONE',  ( -0.7071067811865437980, 0.000000000000000000, -0.7071067811865512365 ) ) ;
#4196 = ORIENTED_EDGE ( 'NONE', *, *, #722, .F. ) ;
#4197 = AXIS2_PLACEMENT_3D ( 'NONE', #3704, #4117, #2607 ) ;
#4198 = ORIENTED_EDGE ( 'NONE', *, *, #3794, .T. ) ;
#4199 = VERTEX_POINT ( 'NONE', #1625 ) ;
#4200 = ORIENTED_EDGE ( 'NONE', *, *, #778, .F. ) ;
#4201 = CARTESIAN_POINT ( 'NONE',  ( 26.49999999999999645, -0.5000000000000000000, 19.50000000000000000 ) ) ;
#4202 = CYLINDRICAL_SURFACE ( 'NONE', #2694, 5.500000000000000000 ) ;
#4203 = ORIENTED_EDGE ( 'NONE', *, *, #2599, .T. ) ;
#4204 = CONICAL_SURFACE ( 'NONE', #1069, 27.99999999999999645, 0.7853981633974457255 ) ;
#4205 = DIRECTION ( 'NONE',  ( 1.000000000000000000, 0.000000000000000000, 0.000000000000000000 ) ) ;
#4206 = CYLINDRICAL_SURFACE ( 'NONE', #1208, 1.749999999999999778 ) ;
#4207 = CYLINDRICAL_SURFACE ( 'NONE', #1257, 4.000000000000000000 ) ;
#4208 = CIRCLE ( 'NONE', #2285, 1.000000000000000888 ) ;
#4209 = EDGE_LOOP ( 'NONE', ( #3376, #2349 ) ) ;
#4210 = AXIS2_PLACEMENT_3D ( 'NONE', #1739, #678, #313 ) ;
#4211 = CARTESIAN_POINT ( 'NONE',  ( 18.35919055844633974, 23.72657184721635204, 10.28976100101469981 ) ) ;
#4212 = EDGE_CURVE ( 'NONE', #2030, #4484, #4510, .T. ) ;
#4213 = CARTESIAN_POINT ( 'NONE',  ( -0.5000000000000000000, 0.000000000000000000, 19.50000000000000000 ) ) ;
#4214 = CARTESIAN_POINT ( 'NONE',  ( -20.28106296843844092, 22.10738654751461851, 5.205249767788494353 ) ) ;
#4215 = DIRECTION ( 'NONE',  ( 0.000000000000000000, 0.000000000000000000, 1.000000000000000000 ) ) ;
#4216 = DIRECTION ( 'NONE',  ( -0.000000000000000000, 1.000000000000000000, -0.000000000000000000 ) ) ;
#4217 = VERTEX_POINT ( 'NONE', #4532 ) ;
#4218 = ORIENTED_EDGE ( 'NONE', *, *, #3334, .T. ) ;
#4219 = EDGE_LOOP ( 'NONE', ( #3099, #3659 ) ) ;
#4220 = DIRECTION ( 'NONE',  ( -1.000000000000000000, 0.000000000000000000, 0.000000000000000000 ) ) ;
#4221 = AXIS2_PLACEMENT_3D ( 'NONE', #1818, #2915, #4368 ) ;
#4222 = DIRECTION ( 'NONE',  ( -0.000000000000000000, -0.000000000000000000, 1.000000000000000000 ) ) ;
#4223 = CARTESIAN_POINT ( 'NONE',  ( 4.020538011569923144E-15, 41.00000000000000000, 12.99999999999999289 ) ) ;
#4224 = AXIS2_PLACEMENT_3D ( 'NONE', #203, #3055, #1302 ) ;
#4225 = CARTESIAN_POINT ( 'NONE',  ( 3.469446951953614189E-15, 33.00000000000000000, 4.999999999999992006 ) ) ;
#4226 =( NAMED_UNIT ( * ) SI_UNIT ( $, .STERADIAN. ) SOLID_ANGLE_UNIT ( ) );
#4227 = CARTESIAN_POINT ( 'NONE',  ( 3.469446951953614189E-15, 30.00000000000000355, 4.999999999999992006 ) ) ;
#4228 = ORIENTED_EDGE ( 'NONE', *, *, #1748, .T. ) ;
#4229 = DIRECTION ( 'NONE',  ( 0.000000000000000000, 0.000000000000000000, 1.000000000000000000 ) ) ;
#4230 =( GEOMETRIC_REPRESENTATION_CONTEXT ( 3 ) GLOBAL_UNCERTAINTY_ASSIGNED_CONTEXT ( ( #4150 ) ) GLOBAL_UNIT_ASSIGNED_CONTEXT ( ( #263, #1379, #3230 ) ) REPRESENTATION_CONTEXT ( 'NONE', 'WORKASPACE' ) );
#4231 = CARTESIAN_POINT ( 'NONE',  ( 21.57966755480319421, 20.84186778456420797, 12.97440020260208193 ) ) ;
#4232 = CARTESIAN_POINT ( 'NONE',  ( 27.09999999999999787, -0.5999999999999998668, 19.59999999999999787 ) ) ;
#4233 = AXIS2_PLACEMENT_3D ( 'NONE', #1307, #4513, #4166 ) ;
#4234 = DIRECTION ( 'NONE',  ( -0.000000000000000000, -1.000000000000000000, -0.000000000000000000 ) ) ;
#4235 = CARTESIAN_POINT ( 'NONE',  ( -5.409090909090905619, 37.00000000000000000, 8.004140804536053366 ) ) ;
#4236 = PLANE ( 'NONE',  #296 ) ;
#4237 = ORIENTED_EDGE ( 'NONE', *, *, #4271, .T. ) ;
#4238 = ORIENTED_EDGE ( 'NONE', *, *, #766, .T. ) ;
#4239 = ORIENTED_EDGE ( 'NONE', *, *, #4058, .F. ) ;
#4240 = PLANE ( 'NONE',  #1655 ) ;
#4241 = FILL_AREA_STYLE_COLOUR ( '', #4578 ) ;
#4242 = EDGE_CURVE ( 'NONE', #468, #1490, #2687, .T. ) ;
#4243 = ADVANCED_FACE ( 'NONE', ( #1649 ), #4207, .F. ) ;
#4244 = DIRECTION ( 'NONE',  ( -0.000000000000000000, 1.000000000000000000, 0.000000000000000000 ) ) ;
#4245 = LINE ( 'NONE', #1346, #1236 ) ;
#4246 = FACE_OUTER_BOUND ( 'NONE', #4074, .T. ) ;
#4247 = AXIS2_PLACEMENT_3D ( 'NONE', #3069, #3328, #4524 ) ;
#4248 = CARTESIAN_POINT ( 'NONE',  ( 1.771177265432712700, 29.94863972218313464, 12.59594310203364387 ) ) ;
#4249 = ORIENTED_EDGE ( 'NONE', *, *, #2021, .T. ) ;
#4250 = CIRCLE ( 'NONE', #3869, 1.750000000000001554 ) ;
#4251 = CARTESIAN_POINT ( 'NONE',  ( 3.469446951953614189E-15, 49.00000000000000000, 8.999999999999992895 ) ) ;
#4252 = CARTESIAN_POINT ( 'NONE',  ( -3.796077574538131660, 29.75903253174124430, 10.28786097927510923 ) ) ;
#4253 = AXIS2_PLACEMENT_3D ( 'NONE', #179, #585, #4581 ) ;
#4254 = CARTESIAN_POINT ( 'NONE',  ( 24.67207871933483432, -8.377607117416795646, 20.00001200000000523 ) ) ;
#4255 = DIRECTION ( 'NONE',  ( 0.000000000000000000, 0.000000000000000000, 1.000000000000000000 ) ) ;
#4256 = DIRECTION ( 'NONE',  ( 0.000000000000000000, -0.000000000000000000, 1.000000000000000000 ) ) ;
#4257 = LINE ( 'NONE', #3896, #2699 ) ;
#4258 = APPLICATION_CONTEXT ( 'automotive_design' ) ;
#4259 = ORIENTED_EDGE ( 'NONE', *, *, #2377, .F. ) ;
#4260 = ORIENTED_EDGE ( 'NONE', *, *, #3561, .T. ) ;
#4261 = CARTESIAN_POINT ( 'NONE',  ( -0.5000000000000000000, 0.000000000000000000, 19.50000000000000000 ) ) ;
#4262 = SURFACE_SIDE_STYLE ('',( #3255 ) ) ;
#4263 = ADVANCED_FACE ( 'NONE', ( #1695 ), #946, .T. ) ;
#4265 = CIRCLE ( 'NONE', #1442, 26.00000000000000711 ) ;
#4264 = SURFACE_SIDE_STYLE ('',( #1736 ) ) ;
#4266 = FACE_OUTER_BOUND ( 'NONE', #170, .T. ) ;
#4267 = DIRECTION ( 'NONE',  ( -0.000000000000000000, 1.000000000000000000, 0.000000000000000000 ) ) ;
#4268 = DIRECTION ( 'NONE',  ( -1.000000000000000000, -0.000000000000000000, -0.000000000000000000 ) ) ;
#4269 = EDGE_CURVE ( 'NONE', #2965, #834, #3910, .T. ) ;
#4270 = FACE_OUTER_BOUND ( 'NONE', #383, .T. ) ;
#4271 = EDGE_CURVE ( 'NONE', #1161, #1870, #1326, .T. ) ;
#4272 = VERTEX_POINT ( 'NONE', #159 ) ;
#4273 = FILL_AREA_STYLE_COLOUR ( '', #4020 ) ;
#4274 = PRODUCT_DEFINITION_SHAPE ( 'NONE', 'NONE',  #2248 ) ;
#4275 = AXIS2_PLACEMENT_3D ( 'NONE', #1171, #4052, #3712 ) ;
#4276 = DIRECTION ( 'NONE',  ( 5.782411586589374402E-16, -1.000000000000000000, 0.000000000000000000 ) ) ;
#4277 = DIRECTION ( 'NONE',  ( 0.7071067811865463515, -0.7071067811865487940, 0.000000000000000000 ) ) ;
#4278 = CARTESIAN_POINT ( 'NONE',  ( -25.99519186311192342, -0.5000000000000000000, 20.00000000000000000 ) ) ;
#4279 = VECTOR ( 'NONE', #789, 1000.000000000000000 ) ;
#4280 = CARTESIAN_POINT ( 'NONE',  ( -22.99914926278833249, 19.26328748721751438, 5.984828968106582714 ) ) ;
#4281 = DIRECTION ( 'NONE',  ( -1.000000000000000000, -0.000000000000000000, -0.000000000000000000 ) ) ;
#4282 = EDGE_CURVE ( 'NONE', #27, #4496, #3125, .T. ) ;
#4283 = CARTESIAN_POINT ( 'NONE',  ( 0.000000000000000000, 0.000000000000000000, 19.50000000000000000 ) ) ;
#4284 = ORIENTED_EDGE ( 'NONE', *, *, #309, .T. ) ;
#4285 = ORIENTED_EDGE ( 'NONE', *, *, #3636, .T. ) ;
#4286 = CYLINDRICAL_SURFACE ( 'NONE', #1359, 24.00000000000000355 ) ;
#4287 = EDGE_CURVE ( 'NONE', #3116, #3925, #3502, .T. ) ;
#4288 =( LENGTH_UNIT ( ) NAMED_UNIT ( * ) SI_UNIT ( .MILLI., .METRE. ) );
#4289 = CARTESIAN_POINT ( 'NONE',  ( 0.000000000000000000, 0.000000000000000000, 0.000000000000000000 ) ) ;
#4290 = PRODUCT_DEFINITION_CONTEXT ( 'detailed design', #4258, 'design' ) ;
#4291 = ORIENTED_EDGE ( 'NONE', *, *, #543, .T. ) ;
#4292 = DIRECTION ( 'NONE',  ( -0.000000000000000000, -1.000000000000000000, -0.000000000000000000 ) ) ;
#4293 = CARTESIAN_POINT ( 'NONE',  ( 3.120626071653185285, 49.00000000000000000, 4.471016347907789346 ) ) ;
#4294 = VECTOR ( 'NONE', #2107, 1000.000000000000114 ) ;
#4295 = DIRECTION ( 'NONE',  ( 1.000000000000000000, 0.000000000000000000, 0.000000000000000000 ) ) ;
#4296 = CARTESIAN_POINT ( 'NONE',  ( 3.973627609689486917, 29.73571816432124493, 9.527501605019752517 ) ) ;
#4297 = CIRCLE ( 'NONE', #4682, 0.7500000000000001110 ) ;
#4298 = MECHANICAL_DESIGN_GEOMETRIC_PRESENTATION_REPRESENTATION (  '', ( #3462 ), #578 ) ;
#4299 = CARTESIAN_POINT ( 'NONE',  ( 3.469446951953614189E-15, 37.00000000000000000, 8.999999999999992895 ) ) ;
#4300 = SHAPE_DEFINITION_REPRESENTATION ( #2823, #3681 ) ;
#4301 = EDGE_CURVE ( 'NONE', #2878, #1161, #4297, .T. ) ;
#4302 = LINE ( 'NONE', #4278, #3929 ) ;
#4303 = ADVANCED_FACE ( 'NONE', ( #4133, #536, #226 ), #2719, .T. ) ;
#4304 = CYLINDRICAL_SURFACE ( 'NONE', #4348, 4.000000000000000000 ) ;
#4305 = DIRECTION ( 'NONE',  ( -0.000000000000000000, -1.000000000000000000, -0.000000000000000000 ) ) ;
#4306 = CARTESIAN_POINT ( 'NONE',  ( 0.000000000000000000, 0.000000000000000000, 15.00000000000000178 ) ) ;
#4307 = CIRCLE ( 'NONE', #205, 4.000000000000000000 ) ;
#4308 = VERTEX_POINT ( 'NONE', #2399 ) ;
#4309 = ORIENTED_EDGE ( 'NONE', *, *, #1762, .T. ) ;
#4310 =( GEOMETRIC_REPRESENTATION_CONTEXT ( 3 ) GLOBAL_UNCERTAINTY_ASSIGNED_CONTEXT ( ( #481 ) ) GLOBAL_UNIT_ASSIGNED_CONTEXT ( ( #3442, #121, #1237 ) ) REPRESENTATION_CONTEXT ( 'NONE', 'WORKASPACE' ) );
#4311 = CARTESIAN_POINT ( 'NONE',  ( 3.959305671612555570E-15, 40.00000000000000000, 4.999999999999990230 ) ) ;
#4312 = CIRCLE ( 'NONE', #2785, 0.5000000000000001110 ) ;
#4313 = CARTESIAN_POINT ( 'NONE',  ( 3.469446951953614189E-15, 41.00000000000000000, 3.999999999999991562 ) ) ;
#4314 = ORIENTED_EDGE ( 'NONE', *, *, #4620, .F. ) ;
#4315 = DIRECTION ( 'NONE',  ( -0.000000000000000000, -0.000000000000000000, -1.000000000000000000 ) ) ;
#4316 = PLANE ( 'NONE',  #2041 ) ;
#4317 = DIRECTION ( 'NONE',  ( 0.000000000000000000, 0.000000000000000000, -1.000000000000000000 ) ) ;
#4318 = CARTESIAN_POINT ( 'NONE',  ( -27.10000000000000497, 0.6000000000000000888, 19.59999999999999787 ) ) ;
#4319 = AXIS2_PLACEMENT_3D ( 'NONE', #3490, #1631, #4591 ) ;
#4320 = CARTESIAN_POINT ( 'NONE',  ( 3.471963499745398973, 32.73349503686927164, 7.013453814050719437 ) ) ;
#4321 = AXIS2_PLACEMENT_3D ( 'NONE', #3540, #2411, #1687 ) ;
#4322 = ADVANCED_FACE ( 'NONE', ( #3460 ), #918, .T. ) ;
#4323 = CARTESIAN_POINT ( 'NONE',  ( -23.72677024356903530, 18.35893773391720529, 7.710863047761279176 ) ) ;
#4324 = DIRECTION ( 'NONE',  ( 0.000000000000000000, 1.000000000000000000, 0.000000000000000000 ) ) ;
#4325 = DIRECTION ( 'NONE',  ( 1.000000000000000000, 0.000000000000000000, 0.000000000000000000 ) ) ;
#4326 = EDGE_CURVE ( 'NONE', #1336, #668, #1026, .T. ) ;
#4327 = ORIENTED_EDGE ( 'NONE', *, *, #932, .T. ) ;
#4328 = ORIENTED_EDGE ( 'NONE', *, *, #1440, .F. ) ;
#4329 = CIRCLE ( 'NONE', #291, 1.000000000000000000 ) ;
#4330 = CARTESIAN_POINT ( 'NONE',  ( 14.84924240491753800, 20.50609665440984841, 8.999999999999992895 ) ) ;
#4331 =( NAMED_UNIT ( * ) SI_UNIT ( $, .STERADIAN. ) SOLID_ANGLE_UNIT ( ) );
#4332 = DIRECTION ( 'NONE',  ( -1.000000000000000000, 0.000000000000000000, 0.000000000000000000 ) ) ;
#4333 = EDGE_LOOP ( 'NONE', ( #1626, #4646, #981, #3639, #4027, #2945, #1591, #124 ) ) ;
#4334 = DIRECTION ( 'NONE',  ( 1.000000000000000000, 0.000000000000000000, 0.000000000000000000 ) ) ;
#4335 = PLANE ( 'NONE',  #2184 ) ;
#4336 = CIRCLE ( 'NONE', #4343, 4.000000000000000000 ) ;
#4337 = PLANE ( 'NONE',  #437 ) ;
#4338 = DIRECTION ( 'NONE',  ( 1.000000000000000000, 0.000000000000000000, 0.000000000000000000 ) ) ;
#4339 = EDGE_CURVE ( 'NONE', #4118, #1513, #3433, .T. ) ;
#4340 =( NAMED_UNIT ( * ) SI_UNIT ( $, .STERADIAN. ) SOLID_ANGLE_UNIT ( ) );
#4341 = CARTESIAN_POINT ( 'NONE',  ( 22.58188871325897296, 19.75109744359741981, 12.47298490618377720 ) ) ;
#4342 = CONTEXT_DEPENDENT_SHAPE_REPRESENTATION ( #3521, #1382 ) ;
#4343 = AXIS2_PLACEMENT_3D ( 'NONE', #470, #4021, #2199 ) ;
#4344 = DIRECTION ( 'NONE',  ( -1.000000000000000000, 0.000000000000000000, 0.000000000000000000 ) ) ;
#4345 = DIRECTION ( 'NONE',  ( 1.000000000000000000, 0.000000000000000000, 0.000000000000000000 ) ) ;
#4346 = CARTESIAN_POINT ( 'NONE',  ( 25.99519186311192342, 0.5000000000000000000, 19.50000000000000000 ) ) ;
#4347 = CLOSED_SHELL ( 'NONE', ( #1280, #4473, #4243, #4095, #3437, #2289, #1878, #392, #2750, #1417, #332, #3831, #4303, #4487, #3044, #4430, #3127, #891, #4655, #2722, #2388, #2502, #1155, #2688, #254, #1215, #914, #624, #1583, #3938, #4162, #1495, #193, #3071, #1617, #1378, #112, #4411 ) ) ;
#4348 = AXIS2_PLACEMENT_3D ( 'NONE', #1044, #4642, #2799 ) ;
#4349 = ORIENTED_EDGE ( 'NONE', *, *, #2027, .F. ) ;
#4350 = ORIENTED_EDGE ( 'NONE', *, *, #4622, .T. ) ;
#4351 = CARTESIAN_POINT ( 'NONE',  ( -3.707290417464794707, 31.67671859859259698, 10.50513240900691159 ) ) ;
#4352 = EDGE_CURVE ( 'NONE', #834, #1922, #412, .T. ) ;
#4353 =( NAMED_UNIT ( * ) SI_UNIT ( $, .STERADIAN. ) SOLID_ANGLE_UNIT ( ) );
#4354 = DIRECTION ( 'NONE',  ( 0.000000000000000000, -1.000000000000000000, -0.000000000000000000 ) ) ;
#4355 = ORIENTED_EDGE ( 'NONE', *, *, #711, .F. ) ;
#4356 = VERTEX_POINT ( 'NONE', #560 ) ;
#4357 = ORIENTED_EDGE ( 'NONE', *, *, #1912, .F. ) ;
#4358 = CARTESIAN_POINT ( 'NONE',  ( 0.000000000000000000, 0.000000000000000000, 19.50000000000000000 ) ) ;
#4359 = CARTESIAN_POINT ( 'NONE',  ( 3.900821110013157789, 34.79398413074517293, 9.893616917921782772 ) ) ;
#4360 = FACE_BOUND ( 'NONE', #1576, .T. ) ;
#4361 = VERTEX_POINT ( 'NONE', #612 ) ;
#4362 = VECTOR ( 'NONE', #2963, 1000.000000000000000 ) ;
#4363 = DIRECTION ( 'NONE',  ( 1.000000000000000000, 0.000000000000000000, 0.000000000000000000 ) ) ;
#4364 = CARTESIAN_POINT ( 'NONE',  ( 0.000000000000000000, 0.000000000000000000, 19.59999999999999787 ) ) ;
#4365 = AXIS2_PLACEMENT_3D ( 'NONE', #4463, #1888, #2961 ) ;
#4366 = AXIS2_PLACEMENT_3D ( 'NONE', #1080, #3984, #726 ) ;
#4367 = DIRECTION ( 'NONE',  ( 0.000000000000000000, 0.000000000000000000, 1.000000000000000000 ) ) ;
#4368 = DIRECTION ( 'NONE',  ( 0.000000000000000000, 0.000000000000000000, 1.000000000000000000 ) ) ;
#4369 = CARTESIAN_POINT ( 'NONE',  ( 3.469446951953614189E-15, 40.00000000000000000, 8.999999999999992895 ) ) ;
#4370 = ORIENTED_EDGE ( 'NONE', *, *, #564, .T. ) ;
#4371 = VERTEX_POINT ( 'NONE', #2008 ) ;
#4372 = CARTESIAN_POINT ( 'NONE',  ( -3.464101615137749501, 32.86558337745499614, 6.999999999999988454 ) ) ;
#4373 = VECTOR ( 'NONE', #3606, 1000.000000000000000 ) ;
#4374 = CARTESIAN_POINT ( 'NONE',  ( 1.000000000000000000, 0.000000000000000000, 19.50000000000000000 ) ) ;
#4375 = ORIENTED_EDGE ( 'NONE', *, *, #4436, .F. ) ;
#4376 = VERTEX_POINT ( 'NONE', #1766 ) ;
#4377 = ORIENTED_EDGE ( 'NONE', *, *, #974, .F. ) ;
#4378 = DIRECTION ( 'NONE',  ( -0.000000000000000000, -1.000000000000000000, 0.000000000000000000 ) ) ;
#4379 = CIRCLE ( 'NONE', #890, 4.000000000000001776 ) ;
#4380 = LINE ( 'NONE', #2536, #824 ) ;
#4381 = CARTESIAN_POINT ( 'NONE',  ( -22.10831845702707454, 20.28006516365564238, 12.79440425686131988 ) ) ;
#4382 = ADVANCED_BREP_SHAPE_REPRESENTATION ( '', ( #2976, #2928 ), #3775 ) ;
#4383 = ADVANCED_FACE ( 'NONE', ( #1811 ), #3379, .T. ) ;
#4384 = EDGE_CURVE ( 'NONE', #2679, #2030, #3537, .T. ) ;
#4385 = CYLINDRICAL_SURFACE ( 'NONE', #1707, 0.5000000000000000000 ) ;
#4386 = CARTESIAN_POINT ( 'NONE',  ( -25.83240171513484285, -3.403349963601435935, 20.00001200000000168 ) ) ;
#4387 = ORIENTED_EDGE ( 'NONE', *, *, #3577, .F. ) ;
#4388 = DIRECTION ( 'NONE',  ( 0.000000000000000000, 0.000000000000000000, 1.000000000000000000 ) ) ;
#4389 = APPLICATION_PROTOCOL_DEFINITION ( 'draft international standard', 'automotive_design', 1998, #3739 ) ;
#4390 = CARTESIAN_POINT ( 'NONE',  ( 21.02954719696287356, 21.39687781493357832, 4.999903794384585431 ) ) ;
#4391 = LINE ( 'NONE', #4417, #2157 ) ;
#4392 = AXIS2_PLACEMENT_3D ( 'NONE', #3428, #859, #838 ) ;
#4393 = CARTESIAN_POINT ( 'NONE',  ( -3.993269581196945417, 34.98663585528726117, 8.733908321742497094 ) ) ;
#4394 = ORIENTED_EDGE ( 'NONE', *, *, #1910, .F. ) ;
#4395 = ORIENTED_EDGE ( 'NONE', *, *, #4384, .F. ) ;
#4396 = AXIS2_PLACEMENT_3D ( 'NONE', #2793, #273, #1721 ) ;
#4397 = CARTESIAN_POINT ( 'NONE',  ( -3.948598437009891882, 31.10436397916096496, 8.348972239903947212 ) ) ;
#4398 =( LENGTH_UNIT ( ) NAMED_UNIT ( * ) SI_UNIT ( .MILLI., .METRE. ) );
#4399 = CARTESIAN_POINT ( 'NONE',  ( 3.469446951953614189E-15, 30.00000000000000355, 8.999999999999992895 ) ) ;
#4400 = ORIENTED_EDGE ( 'NONE', *, *, #3393, .F. ) ;
#4401 = VERTEX_POINT ( 'NONE', #1717 ) ;
#4402 = AXIS2_PLACEMENT_3D ( 'NONE', #831, #3750, #1563 ) ;
#4403 = EDGE_LOOP ( 'NONE', ( #478, #258, #1570, #1508 ) ) ;
#4404 = LINE ( 'NONE', #3594, #1285 ) ;
#4405 = EDGE_CURVE ( 'NONE', #1759, #3886, #1410, .T. ) ;
#4406 = CARTESIAN_POINT ( 'NONE',  ( 3.469446951953614189E-15, 25.00000000000000000, 8.999999999999992895 ) ) ;
#4407 = CARTESIAN_POINT ( 'NONE',  ( 0.7500000000000000000, -1.299038105676658450, 17.69999999999999929 ) ) ;
#4408 = CARTESIAN_POINT ( 'NONE',  ( -11.52193136556784658, -23.36965697125209118, 20.00001200000000168 ) ) ;
#4409 = ORIENTED_EDGE ( 'NONE', *, *, #4554, .F. ) ;
#4410 =( REPRESENTATION_RELATIONSHIP ('NONE','NONE', #2397, #1892 ) REPRESENTATION_RELATIONSHIP_WITH_TRANSFORMATION ( #1746 )SHAPE_REPRESENTATION_RELATIONSHIP( ) );
#4411 = ADVANCED_FACE ( 'NONE', ( #4270 ), #3907, .T. ) ;
#4412 = FILL_AREA_STYLE_COLOUR ( '', #2877 ) ;
#4413 = EDGE_CURVE ( 'NONE', #2385, #3258, #3456, .T. ) ;
#4414 = FACE_OUTER_BOUND ( 'NONE', #1514, .T. ) ;
#4415 = VECTOR ( 'NONE', #123, 1000.000000000000000 ) ;
#4416 = CARTESIAN_POINT ( 'NONE',  ( 20.28368189782986519, 22.10500230410270106, 5.203924605526645486 ) ) ;
#4417 = CARTESIAN_POINT ( 'NONE',  ( 0.5000000000000000000, -2.999999999999999556, 20.00000000000000000 ) ) ;
#4418 = CARTESIAN_POINT ( 'NONE',  ( -3.948285692887619991, 34.89498999672885304, 9.652966208173760165 ) ) ;
#4419 = ORIENTED_EDGE ( 'NONE', *, *, #2632, .F. ) ;
#4420 = ORIENTED_EDGE ( 'NONE', *, *, #1647, .T. ) ;
#4421 = CARTESIAN_POINT ( 'NONE',  ( 3.469446951953614189E-15, 49.00000000000000000, 8.999999999999992895 ) ) ;
#4422 = AXIS2_PLACEMENT_3D ( 'NONE', #3357, #2613, #1547 ) ;
#4423 = DIRECTION ( 'NONE',  ( 0.000000000000000000, 1.000000000000000000, 0.000000000000000000 ) ) ;
#4424 = ORIENTED_EDGE ( 'NONE', *, *, #1620, .F. ) ;
#4425 = ORIENTED_EDGE ( 'NONE', *, *, #364, .T. ) ;
#4426 = ORIENTED_EDGE ( 'NONE', *, *, #2021, .F. ) ;
#4427 = EDGE_CURVE ( 'NONE', #3785, #29, #3989, .T. ) ;
#4428 = CARTESIAN_POINT ( 'NONE',  ( -26.50000000000000355, 0.5000000000000000000, 19.00000000000000000 ) ) ;
#4429 = CARTESIAN_POINT ( 'NONE',  ( -21.93582988124917321, 20.46667490424612268, 12.87153294081770483 ) ) ;
#4430 = ADVANCED_FACE ( 'NONE', ( #3937 ), #681, .F. ) ;
#4431 = CARTESIAN_POINT ( 'NONE',  ( -0.7500000000000001110, 9.184850993605150903E-17, 15.00000000000000178 ) ) ;
#4432 = CARTESIAN_POINT ( 'NONE',  ( 3.889087296526035242, 37.00000000000000000, 5.110912703473999841 ) ) ;
#4433 = ORIENTED_EDGE ( 'NONE', *, *, #3978, .T. ) ;
#4434 = FACE_OUTER_BOUND ( 'NONE', #1491, .T. ) ;
#4435 = CARTESIAN_POINT ( 'NONE',  ( 3.464101615137757495, 33.00000000000000000, 10.99999999999999467 ) ) ;
#4436 = EDGE_CURVE ( 'NONE', #1896, #2610, #3151, .T. ) ;
#4437 = EDGE_CURVE ( 'NONE', #3868, #4670, #3620, .T. ) ;
#4438 = CARTESIAN_POINT ( 'NONE',  ( 18.35893773391728701, 23.72677024356898201, 7.710863047761277400 ) ) ;
#4439 = AXIS2_PLACEMENT_3D ( 'NONE', #3316, #873, #2941 ) ;
#4440 = DIRECTION ( 'NONE',  ( -0.000000000000000000, 1.000000000000000000, -0.000000000000000000 ) ) ;
#4441 = DIRECTION ( 'NONE',  ( 0.000000000000000000, 0.000000000000000000, 1.000000000000000000 ) ) ;
#4442 = MANIFOLD_SOLID_BREP ( 'Chamfer1', #1917 ) ;
#4443 = ORIENTED_EDGE ( 'NONE', *, *, #3393, .T. ) ;
#4444 = ORIENTED_EDGE ( 'NONE', *, *, #3432, .F. ) ;
#4445 = AXIS2_PLACEMENT_3D ( 'NONE', #3967, #2886, #1014 ) ;
#4446 = ADVANCED_FACE ( 'NONE', ( #382 ), #4385, .T. ) ;
#4447 = CARTESIAN_POINT ( 'NONE',  ( -3.575798854573970509, 32.10535367473890744, 10.79358726550605851 ) ) ;
#4448 = CARTESIAN_POINT ( 'NONE',  ( 0.000000000000000000, 0.000000000000000000, 16.00000000000000000 ) ) ;
#4449 = SURFACE_STYLE_USAGE ( .BOTH. , #1824 ) ;
#4450 = CYLINDRICAL_SURFACE ( 'NONE', #2130, 1.000000000000000888 ) ;
#4451 = ORIENTED_EDGE ( 'NONE', *, *, #1871, .F. ) ;
#4452 = ORIENTED_EDGE ( 'NONE', *, *, #3188, .F. ) ;
#4453 = ORIENTED_EDGE ( 'NONE', *, *, #3981, .F. ) ;
#4454 = ORIENTED_EDGE ( 'NONE', *, *, #4301, .T. ) ;
#4455 = UNCERTAINTY_MEASURE_WITH_UNIT (LENGTH_MEASURE( 1.000000000000000082E-05 ), #1961, 'distance_accuracy_value', 'NONE');
#4456 = CARTESIAN_POINT ( 'NONE',  ( 27.17157287525387588, 32.82842712474614189, 8.999999999999992895 ) ) ;
#4457 = CARTESIAN_POINT ( 'NONE',  ( 3.469446951953614189E-15, 34.00000000000000000, 8.999999999999992895 ) ) ;
#4458 = DIRECTION ( 'NONE',  ( 0.000000000000000000, 0.000000000000000000, 1.000000000000000000 ) ) ;
#4459 = PRODUCT_DEFINITION_SHAPE ( 'NONE', 'NONE',  #4709 ) ;
#4460 = VERTEX_POINT ( 'NONE', #1496 ) ;
#4461 = VECTOR ( 'NONE', #594, 1000.000000000000000 ) ;
#4462 = CARTESIAN_POINT ( 'NONE',  ( -0.9958591954639161026, 43.00000000000000000, 3.590909090909080170 ) ) ;
#4463 = CARTESIAN_POINT ( 'NONE',  ( 0.000000000000000000, 0.000000000000000000, 19.59999999999999787 ) ) ;
#4464 = B_SPLINE_CURVE_WITH_KNOTS ( 'NONE', 3,
 ( #1584, #1309, #1992, #519, #4492, #185, #567, #3419, #2751, #1262, #2312, #4139, #2700, #4214, #875, #4167, #3780, #2380, #595, #2040, #3489, #2106, #301, #1418, #4280, #3945, #1771, #665, #3511, #4323, #1751, #3199, #1017, #618 ),
 .UNSPECIFIED., .F., .F.,
 ( 4, 2, 2, 2, 2, 2, 2, 2, 2, 2, 2, 2, 2, 2, 2, 2, 4 ),
 ( 0.000000000000000000, 0.0007824845743203488312, 0.001564969148640697662, 0.002347453722961046277, 0.003129938297281395325, 0.003912422871601744373, 0.004694907445922092554, 0.005477392020242441602, 0.006259876594562790650, 0.007042361168883139698, 0.007824845743203488746, 0.008607330317523836927, 0.009389814891844185107, 0.01017229946616453502, 0.01095478404048488320, 0.01173726861480523312, 0.01251975318912558130 ),
 .UNSPECIFIED. ) ;
#4465 = EDGE_CURVE ( 'NONE', #4120, #4100, #3677, .T. ) ;
#4466 = CARTESIAN_POINT ( 'NONE',  ( 0.000000000000000000, 0.000000000000000000, 20.00000000000000000 ) ) ;
#4467 = DIRECTION ( 'NONE',  ( 0.000000000000000000, -0.000000000000000000, 1.000000000000000000 ) ) ;
#4468 = VERTEX_POINT ( 'NONE', #3359 ) ;
#4469 = EDGE_CURVE ( 'NONE', #1957, #2969, #2541, .T. ) ;
#4470 = DIRECTION ( 'NONE',  ( 0.000000000000000000, 0.000000000000000000, 1.000000000000000000 ) ) ;
#4471 = CIRCLE ( 'NONE', #4181, 4.750000000000002665 ) ;
#4472 = PLANE ( 'NONE',  #2108 ) ;
#4473 = ADVANCED_FACE ( 'NONE', ( #2565, #3642, #4360, #1831 ), #4107, .T. ) ;
#4474 = CARTESIAN_POINT ( 'NONE',  ( 0.000000000000000000, 0.000000000000000000, 0.000000000000000000 ) ) ;
#4475 = LINE ( 'NONE', #4141, #307 ) ;
#4476 = ORIENTED_EDGE ( 'NONE', *, *, #3939, .T. ) ;
#4477 = ORIENTED_EDGE ( 'NONE', *, *, #4037, .T. ) ;
#4478 = ORIENTED_EDGE ( 'NONE', *, *, #2139, .T. ) ;
#4479 = ORIENTED_EDGE ( 'NONE', *, *, #1912, .T. ) ;
#4480 = PRESENTATION_LAYER_ASSIGNMENT (  '', '', ( #754 ) ) ;
#4481 = CARTESIAN_POINT ( 'NONE',  ( 3.469446951953614189E-15, 25.00000000000000000, 4.999999999999992006 ) ) ;
#4482 = UNCERTAINTY_MEASURE_WITH_UNIT (LENGTH_MEASURE( 1.000000000000000082E-05 ), #3954, 'distance_accuracy_value', 'NONE');
#4483 = AXIS2_PLACEMENT_3D ( 'NONE', #1965, #2007, #3459 ) ;
#4484 = VERTEX_POINT ( 'NONE', #3664 ) ;
#4485 = CARTESIAN_POINT ( 'NONE',  ( 0.5000000000000000000, 0.000000000000000000, 20.00000000000000000 ) ) ;
#4486 = FACE_OUTER_BOUND ( 'NONE', #636, .T. ) ;
#4487 = ADVANCED_FACE ( 'NONE', ( #405 ), #2975, .F. ) ;
#4488 = EDGE_CURVE ( 'NONE', #2610, #1290, #841, .T. ) ;
#4489 = AXIS2_PLACEMENT_3D ( 'NONE', #286, #671, #4672 ) ;
#4490 = CARTESIAN_POINT ( 'NONE',  ( -2.644755406393140440, 29.88376691385261097, 5.987824696368042154 ) ) ;
#4491 = CARTESIAN_POINT ( 'NONE',  ( 26.49999999999999645, 0.5000000000000000000, 19.50000000000000000 ) ) ;
#4492 = CARTESIAN_POINT ( 'NONE',  ( -18.35933649373370358, 23.72646225117216900, 7.709376215153277201 ) ) ;
#4493 = FACE_OUTER_BOUND ( 'NONE', #2423, .T. ) ;
#4494 = PRODUCT_DEFINITION_SHAPE ( 'NONE', 'NONE',  #487 ) ;
#4495 = CARTESIAN_POINT ( 'NONE',  ( 3.464101615137757495, 33.00000000000000000, 10.99999999999999467 ) ) ;
#4496 = VERTEX_POINT ( 'NONE', #4407 ) ;
#4497 = ORIENTED_EDGE ( 'NONE', *, *, #693, .F. ) ;
#4498 = VERTEX_POINT ( 'NONE', #4053 ) ;
#4499 = EDGE_LOOP ( 'NONE', ( #475, #3635, #4694, #4357 ) ) ;
#4500 = DIRECTION ( 'NONE',  ( 0.000000000000000000, 0.000000000000000000, -1.000000000000000000 ) ) ;
#4501 = VECTOR ( 'NONE', #3742, 1000.000000000000000 ) ;
#4502 = EDGE_CURVE ( 'NONE', #27, #2849, #2234, .T. ) ;
#4503 = CARTESIAN_POINT ( 'NONE',  ( 26.00000000000000355, 3.184081677783117796E-15, 20.00001200000000168 ) ) ;
#4504 = PRESENTATION_STYLE_ASSIGNMENT (( #1320 ) ) ;
#4505 = CARTESIAN_POINT ( 'NONE',  ( 3.469446951953614189E-15, 49.00000000000000000, 8.999999999999992895 ) ) ;
#4506 = VECTOR ( 'NONE', #4553, 1000.000000000000000 ) ;
#4507 = CARTESIAN_POINT ( 'NONE',  ( 3.469446951953614189E-15, 49.00000000000000000, 8.999999999999992895 ) ) ;
#4508 = LINE ( 'NONE', #2619, #1233 ) ;
#4509 = FACE_OUTER_BOUND ( 'NONE', #4606, .T. ) ;
#4510 = LINE ( 'NONE', #4227, #2085 ) ;
#4511 = VERTEX_POINT ( 'NONE', #1521 ) ;
#4512 = CARTESIAN_POINT ( 'NONE',  ( 0.7500000000000000000, 0.000000000000000000, 17.69999999999999929 ) ) ;
#4513 = DIRECTION ( 'NONE',  ( 0.000000000000000000, 0.000000000000000000, 1.000000000000000000 ) ) ;
#4514 = AXIS2_PLACEMENT_3D ( 'NONE', #1045, #3650, #369 ) ;
#4515 = CARTESIAN_POINT ( 'NONE',  ( 0.000000000000000000, 0.000000000000000000, 17.00000000000000000 ) ) ;
#4516 = CARTESIAN_POINT ( 'NONE',  ( 3.810302108970986978, 34.59594724063161664, 7.767247897849999028 ) ) ;
#4517 = CARTESIAN_POINT ( 'NONE',  ( 0.000000000000000000, 0.000000000000000000, 0.000000000000000000 ) ) ;
#4518 = DIRECTION ( 'NONE',  ( -0.000000000000000000, -1.000000000000000000, -0.000000000000000000 ) ) ;
#4519 = ORIENTED_EDGE ( 'NONE', *, *, #1790, .F. ) ;
#4520 = AXIS2_PLACEMENT_3D ( 'NONE', #1966, #4605, #4157 ) ;
#4521 = ORIENTED_EDGE ( 'NONE', *, *, #469, .T. ) ;
#4522 = VERTEX_POINT ( 'NONE', #1909 ) ;
#4523 = VERTEX_POINT ( 'NONE', #4431 ) ;
#4524 = DIRECTION ( 'NONE',  ( 0.7071067811865462405, -0.7071067811865487940, 0.000000000000000000 ) ) ;
#4525 = CARTESIAN_POINT ( 'NONE',  ( -3.464101615137750390, 33.00000000000000000, 10.99999999999999467 ) ) ;
#4526 = VECTOR ( 'NONE', #4222, 1000.000000000000000 ) ;
#4527 =( NAMED_UNIT ( * ) SI_UNIT ( $, .STERADIAN. ) SOLID_ANGLE_UNIT ( ) );
#4528 = DIRECTION ( 'NONE',  ( 0.000000000000000000, 0.7071067811865451302, 0.7071067811865500152 ) ) ;
#4529 = LINE ( 'NONE', #2736, #2501 ) ;
#4530 = DIRECTION ( 'NONE',  ( 0.000000000000000000, -1.000000000000000000, 0.000000000000000000 ) ) ;
#4531 = EDGE_CURVE ( 'NONE', #786, #2854, #4078, .T. ) ;
#4532 = CARTESIAN_POINT ( 'NONE',  ( 0.5000000000000001110, 6.123233995736767268E-17, 19.50000000000000000 ) ) ;
#4533 = ORIENTED_EDGE ( 'NONE', *, *, #4190, .T. ) ;
#4534 = CIRCLE ( 'NONE', #1038, 1.000000000000000000 ) ;
#4535 = AXIS2_PLACEMENT_3D ( 'NONE', #308, #3257, #3210 ) ;
#4536 = CARTESIAN_POINT ( 'NONE',  ( 18.21571070649545732, 23.83674813237291090, 9.520895848189299571 ) ) ;
#4537 = DIRECTION ( 'NONE',  ( 0.000000000000000000, 1.000000000000000000, 0.000000000000000000 ) ) ;
#4538 = CARTESIAN_POINT ( 'NONE',  ( 0.5000000000000001110, 10.00000000000000000, 13.00000000000000178 ) ) ;
#4539 = CARTESIAN_POINT ( 'NONE',  ( -5.377642775528101993E-14, 49.00000000000000000, 14.49999999999999289 ) ) ;
#4540 = CARTESIAN_POINT ( 'NONE',  ( 0.000000000000000000, 0.000000000000000000, 19.00000000000000000 ) ) ;
#4541 = ORIENTED_EDGE ( 'NONE', *, *, #1070, .F. ) ;
#4542 = ORIENTED_EDGE ( 'NONE', *, *, #1586, .T. ) ;
#4543 = EDGE_LOOP ( 'NONE', ( #2326, #483, #4309, #572, #1904, #835, #3212, #2754 ) ) ;
#4544 = ORIENTED_EDGE ( 'NONE', *, *, #3246, .T. ) ;
#4545 = AXIS2_PLACEMENT_3D ( 'NONE', #2666, #867, #2304 ) ;
#4546 = CARTESIAN_POINT ( 'NONE',  ( 8.999999999999984013, 32.99999999999999289, 0.000000000000000000 ) ) ;
#4547 = CARTESIAN_POINT ( 'NONE',  ( 0.000000000000000000, 0.000000000000000000, 20.00000000000000000 ) ) ;
#4548 = CARTESIAN_POINT ( 'NONE',  ( 0.000000000000000000, 10.00000000000000000, 15.00000000000000178 ) ) ;
#4549 = AXIS2_PLACEMENT_3D ( 'NONE', #1220, #2639, #3377 ) ;
#4550 = ORIENTED_EDGE ( 'NONE', *, *, #4413, .F. ) ;
#4551 = EDGE_CURVE ( 'NONE', #2338, #2965, #1198, .T. ) ;
#4552 = ADVANCED_BREP_SHAPE_REPRESENTATION ( '', ( #1329, #2928 ), #4230 ) ;
#4553 = DIRECTION ( 'NONE',  ( -0.000000000000000000, -1.000000000000000000, -0.000000000000000000 ) ) ;
#4554 = EDGE_CURVE ( 'NONE', #788, #1550, #482, .T. ) ;
#4555 = AXIS2_PLACEMENT_3D ( 'NONE', #3644, #435, #1886 ) ;
#4556 = MANIFOLD_SOLID_BREP ( 'Extrude-Thin1', #4044 ) ;
#4557 = CARTESIAN_POINT ( 'NONE',  ( 0.5000000000000000000, 0.8660254037844387076, 19.50000000000000000 ) ) ;
#4558 = FACE_OUTER_BOUND ( 'NONE', #700, .T. ) ;
#4559 = ORIENTED_EDGE ( 'NONE', *, *, #4269, .F. ) ;
#4560 = EDGE_CURVE ( 'NONE', #4118, #4099, #2379, .T. ) ;
#4561 = CIRCLE ( 'NONE', #3560, 0.5000000000000001110 ) ;
#4562 = ADVANCED_FACE ( 'NONE', ( #940 ), #4202, .T. ) ;
#4563 = CIRCLE ( 'NONE', #3415, 0.9999999999999997780 ) ;
#4564 = DIRECTION ( 'NONE',  ( 0.000000000000000000, 0.000000000000000000, 1.000000000000000000 ) ) ;
#4565 = LINE ( 'NONE', #1970, #808 ) ;
#4566 = AXIS2_PLACEMENT_3D ( 'NONE', #930, #4569, #953 ) ;
#4567 = FACE_OUTER_BOUND ( 'NONE', #1820, .T. ) ;
#4568 = CARTESIAN_POINT ( 'NONE',  ( -26.50000000000000355, -0.5000000000000000000, 19.50000000000000000 ) ) ;
#4569 = DIRECTION ( 'NONE',  ( 0.7071067811865487940, -0.7071067811865463515, 0.000000000000000000 ) ) ;
#4570 = ORIENTED_EDGE ( 'NONE', *, *, #2142, .F. ) ;
#4571 = AXIS2_PLACEMENT_3D ( 'NONE', #2582, #2653, #3038 ) ;
#4572 = EDGE_LOOP ( 'NONE', ( #1895, #1987, #2658, #856 ) ) ;
#4573 = ORIENTED_EDGE ( 'NONE', *, *, #4339, .T. ) ;
#4574 = CARTESIAN_POINT ( 'NONE',  ( 1.500000000000000222, 0.000000000000000000, 18.19999999999999929 ) ) ;
#4575 = CARTESIAN_POINT ( 'NONE',  ( 26.49999999999999645, 0.5000000000000000000, 19.50000000000000000 ) ) ;
#4576 = LINE ( 'NONE', #2761, #4526 ) ;
#4577 = CARTESIAN_POINT ( 'NONE',  ( 3.469446951953614189E-15, 34.00000000000000000, 3.999999999999991562 ) ) ;
#4578 = COLOUR_RGB ( '',0.8941176470588234615, 0.8941176470588234615, 0.8941176470588234615 ) ;
#4579 = CARTESIAN_POINT ( 'NONE',  ( -5.377642775528101993E-14, 34.17157287525380838, 14.49999999999999289 ) ) ;
#4580 = EDGE_CURVE ( 'NONE', #2044, #2022, #3226, .T. ) ;
#4581 = DIRECTION ( 'NONE',  ( 1.000000000000000000, 0.000000000000000000, -0.000000000000000000 ) ) ;
#4582 = CARTESIAN_POINT ( 'NONE',  ( 25.99307600111999150, -0.5999999999999998668, 20.00001200000000168 ) ) ;
#4583 = ORIENTED_EDGE ( 'NONE', *, *, #1869, .T. ) ;
#4584 = CARTESIAN_POINT ( 'NONE',  ( 0.000000000000000000, 0.000000000000000000, 20.00000000000000000 ) ) ;
#4585 = DIRECTION ( 'NONE',  ( 0.7071067811865536790, 0.000000000000000000, -0.7071067811865415775 ) ) ;
#4586 = LINE ( 'NONE', #2038, #3616 ) ;
#4587 = EDGE_CURVE ( 'NONE', #3924, #1957, #3528, .T. ) ;
#4588 = EDGE_CURVE ( 'NONE', #2553, #3303, #2685, .T. ) ;
#4589 = EDGE_CURVE ( 'NONE', #2288, #907, #2013, .T. ) ;
#4590 = DIRECTION ( 'NONE',  ( 0.000000000000000000, 0.000000000000000000, 1.000000000000000000 ) ) ;
#4591 = DIRECTION ( 'NONE',  ( 1.000000000000000000, 0.000000000000000000, 0.000000000000000000 ) ) ;
#4592 = DIRECTION ( 'NONE',  ( -0.000000000000000000, 1.000000000000000000, -0.000000000000000000 ) ) ;
#4593 = ORIENTED_EDGE ( 'NONE', *, *, #897, .T. ) ;
#4594 = ORIENTED_EDGE ( 'NONE', *, *, #250, .T. ) ;
#4595 = VERTEX_POINT ( 'NONE', #4180 ) ;
#4596 = DIRECTION ( 'NONE',  ( -1.000000000000000000, 0.000000000000000000, 0.000000000000000000 ) ) ;
#4597 = CARTESIAN_POINT ( 'NONE',  ( 3.469446951953614189E-15, 49.00000000000000000, 8.999999999999992895 ) ) ;
#4598 = SURFACE_STYLE_FILL_AREA ( #2683 ) ;
#4599 = AXIS2_PLACEMENT_3D ( 'NONE', #3341, #1483, #1504 ) ;
#4600 = DIRECTION ( 'NONE',  ( -1.000000000000000000, 0.000000000000000000, 0.000000000000000000 ) ) ;
#4601 = PLANE ( 'NONE',  #3117 ) ;
#4602 = AXIS2_PLACEMENT_3D ( 'NONE', #3263, #2468, #1431 ) ;
#4603 = DIRECTION ( 'NONE',  ( 1.000000000000000000, 0.000000000000000000, 0.000000000000000000 ) ) ;
#4604 = CARTESIAN_POINT ( 'NONE',  ( 0.5000000000000000000, -2.999999999999999556, 20.00000000000000000 ) ) ;
#4605 = DIRECTION ( 'NONE',  ( -1.927470528863123239E-16, 1.000000000000000000, 0.000000000000000000 ) ) ;
#4606 = EDGE_LOOP ( 'NONE', ( #284, #869 ) ) ;
#4607 = AXIS2_PLACEMENT_3D ( 'NONE', #3143, #2072, #3931 ) ;
#4608 = DIRECTION ( 'NONE',  ( 0.000000000000000000, 0.000000000000000000, 1.000000000000000000 ) ) ;
#4609 = CIRCLE ( 'NONE', #1792, 1.000000000000000000 ) ;
#4610 = CARTESIAN_POINT ( 'NONE',  ( -3.470226642398214878, 29.79897209676519765, 11.00633161724385900 ) ) ;
#4611 = DIRECTION ( 'NONE',  ( 0.000000000000000000, 0.000000000000000000, 1.000000000000000000 ) ) ;
#4612 = PRODUCT_DEFINITION_FORMATION_WITH_SPECIFIED_SOURCE ( 'ANY', '', #3774, .NOT_KNOWN. ) ;
#4613 = CIRCLE ( 'NONE', #2314, 4.000000000000000000 ) ;
#4614 = EDGE_CURVE ( 'NONE', #3335, #3729, #1621, .T. ) ;
#4615 = DIRECTION ( 'NONE',  ( -1.000000000000000000, 0.000000000000000000, 0.000000000000000000 ) ) ;
#4616 = DIRECTION ( 'NONE',  ( 1.000000000000000000, 0.000000000000000000, 0.000000000000000000 ) ) ;
#4617 = DIRECTION ( 'NONE',  ( 0.000000000000000000, 0.000000000000000000, 1.000000000000000000 ) ) ;
#4618 = VERTEX_POINT ( 'NONE', #1321 ) ;
#4619 = ORIENTED_EDGE ( 'NONE', *, *, #2395, .F. ) ;
#4620 = EDGE_CURVE ( 'NONE', #4618, #1239, #3301, .T. ) ;
#4621 = CARTESIAN_POINT ( 'NONE',  ( 0.000000000000000000, 0.000000000000000000, 19.00000000000000000 ) ) ;
#4622 = EDGE_CURVE ( 'NONE', #1560, #2878, #1665, .T. ) ;
#4623 = DIRECTION ( 'NONE',  ( 0.000000000000000000, -0.000000000000000000, 1.000000000000000000 ) ) ;
#4624 = FILL_AREA_STYLE_COLOUR ( '', #1559 ) ;
#4625 =( NAMED_UNIT ( * ) PLANE_ANGLE_UNIT ( ) SI_UNIT ( $, .RADIAN. ) );
#4626 = PRODUCT_DEFINITION_CONTEXT ( 'detailed design', #2515, 'design' ) ;
#4627 = DIRECTION ( 'NONE',  ( 0.000000000000000000, 0.000000000000000000, 1.000000000000000000 ) ) ;
#4628 = DIRECTION ( 'NONE',  ( -0.000000000000000000, -0.000000000000000000, 1.000000000000000000 ) ) ;
#4629 = CARTESIAN_POINT ( 'NONE',  ( -5.409090909090905619, 43.00000000000000000, 8.004140804536053366 ) ) ;
#4630 = VECTOR ( 'NONE', #2459, 1000.000000000000000 ) ;
#4631 = CARTESIAN_POINT ( 'NONE',  ( 1.295195626368611075, 29.97299535330734699, 5.206545655307601272 ) ) ;
#4632 = EDGE_LOOP ( 'NONE', ( #720, #449, #1071, #78 ) ) ;
#4633 = DIRECTION ( 'NONE',  ( 1.000000000000000000, -8.560005772541128451E-15, 0.000000000000000000 ) ) ;
#4634 = EDGE_CURVE ( 'NONE', #3829, #2196, #3607, .T. ) ;
#4635 = CARTESIAN_POINT ( 'NONE',  ( 23.52435923723758648, 18.61790092284045883, 11.00811882721853330 ) ) ;
#4636 = DIRECTION ( 'NONE',  ( 0.000000000000000000, 0.000000000000000000, 1.000000000000000000 ) ) ;
#4637 = FACE_OUTER_BOUND ( 'NONE', #4024, .T. ) ;
#4638 = VECTOR ( 'NONE', #1387, 1000.000000000000000 ) ;
#4639 = EDGE_CURVE ( 'NONE', #4523, #2288, #4576, .T. ) ;
#4640 = AXIS2_PLACEMENT_3D ( 'NONE', #4507, #1251, #581 ) ;
#4641 = SHAPE_REPRESENTATION ( 'ring', ( #2928 ), #3775 ) ;
#4642 = DIRECTION ( 'NONE',  ( -0.000000000000000000, -1.000000000000000000, -0.000000000000000000 ) ) ;
#4643 = DIRECTION ( 'NONE',  ( -0.000000000000000000, -1.000000000000000000, -0.000000000000000000 ) ) ;
#4644 = CARTESIAN_POINT ( 'NONE',  ( -3.809991693235069476, 34.59507057476615444, 7.766500207085086593 ) ) ;
#4645 = ORIENTED_EDGE ( 'NONE', *, *, #804, .T. ) ;
#4646 = ORIENTED_EDGE ( 'NONE', *, *, #1249, .T. ) ;
#4647 = CARTESIAN_POINT ( 'NONE',  ( 27.09999999999999787, 0.6000000000000000888, 19.00000000000000000 ) ) ;
#4648 = DIRECTION ( 'NONE',  ( 0.000000000000000000, 0.000000000000000000, -1.000000000000000000 ) ) ;
#4649 = CONICAL_SURFACE ( 'NONE', #1983, 27.99999999999999645, 0.7853981633974457255 ) ;
#4650 = CYLINDRICAL_SURFACE ( 'NONE', #1784, 1.000000000000000000 ) ;
#4651 = ORIENTED_EDGE ( 'NONE', *, *, #3146, .T. ) ;
#4652 = CARTESIAN_POINT ( 'NONE',  ( 24.67207871933482011, 8.377607117416825844, 20.00001200000000168 ) ) ;
#4653 = ADVANCED_FACE ( 'NONE', ( #964 ), #2393, .F. ) ;
#4654 = LINE ( 'NONE', #2789, #941 ) ;
#4655 = ADVANCED_FACE ( 'NONE', ( #1575 ), #3025, .T. ) ;
#4656 = DIRECTION ( 'NONE',  ( 0.000000000000000000, -0.000000000000000000, 1.000000000000000000 ) ) ;
#4657 = CARTESIAN_POINT ( 'NONE',  ( 3.794405662118193856, 29.75924672568546114, 10.29276539630767573 ) ) ;
#4658 = SURFACE_SIDE_STYLE ('',( #298 ) ) ;
#4659 = PRODUCT_DEFINITION_SHAPE ( 'NONE', 'NONE',  #4715 ) ;
#4660 = AXIS2_PLACEMENT_3D ( 'NONE', #2394, #2714, #2370 ) ;
#4661 = AXIS2_PLACEMENT_3D ( 'NONE', #234, #3134, #2151 ) ;
#4662 = CARTESIAN_POINT ( 'NONE',  ( 3.523144759583864527, 32.34704090027811674, 7.105089090000585195 ) ) ;
#4663 = SHAPE_DEFINITION_REPRESENTATION ( #928, #404 ) ;
#4664 = CARTESIAN_POINT ( 'NONE',  ( 0.000000000000000000, 0.000000000000000000, 0.000000000000000000 ) ) ;
#4665 = CIRCLE ( 'NONE', #2670, 1.000000000000000000 ) ;
#4666 = AXIS2_PLACEMENT_3D ( 'NONE', #3544, #4244, #1406 ) ;
#4667 = CARTESIAN_POINT ( 'NONE',  ( 11.99999999999999822, 45.00000000000000000, 0.000000000000000000 ) ) ;
#4668 = CARTESIAN_POINT ( 'NONE',  ( 3.469446951953614189E-15, 49.00000000000000000, 8.999999999999992895 ) ) ;
#4669 = DIRECTION ( 'NONE',  ( -0.000000000000000000, -0.000000000000000000, -1.000000000000000000 ) ) ;
#4670 = VERTEX_POINT ( 'NONE', #4673 ) ;
#4671 = ORIENTED_EDGE ( 'NONE', *, *, #4551, .F. ) ;
#4672 = DIRECTION ( 'NONE',  ( 0.000000000000000000, 0.000000000000000000, -1.000000000000000000 ) ) ;
#4673 = CARTESIAN_POINT ( 'NONE',  ( -5.409090909090905619, 37.00000000000000000, 9.995859195463932423 ) ) ;
#4674 = FACE_OUTER_BOUND ( 'NONE', #4121, .T. ) ;
#4675 = EDGE_LOOP ( 'NONE', ( #1590, #2603, #3091, #1822 ) ) ;
#4676 = CARTESIAN_POINT ( 'NONE',  ( -24.00000000000000355, 2.939152317953648289E-15, 17.00000000000000000 ) ) ;
#4677 = DIRECTION ( 'NONE',  ( 0.000000000000000000, 0.000000000000000000, 1.000000000000000000 ) ) ;
#4678 = ADVANCED_BREP_SHAPE_REPRESENTATION ( '', ( #4556, #2928 ), #3465 ) ;
#4679 = CIRCLE ( 'NONE', #794, 30.00000000000000355 ) ;
#4680 = CARTESIAN_POINT ( 'NONE',  ( 0.000000000000000000, 0.000000000000000000, 19.50000000000000000 ) ) ;
#4681 = CARTESIAN_POINT ( 'NONE',  ( 1.776153951180677870, 29.94834318124550165, 5.406519136333786335 ) ) ;
#4682 = AXIS2_PLACEMENT_3D ( 'NONE', #512, #3412, #3481 ) ;
#4683 = EDGE_CURVE ( 'NONE', #3492, #4356, #1943, .T. ) ;
#4684 = DIRECTION ( 'NONE',  ( 0.000000000000000000, 1.000000000000000000, 0.000000000000000000 ) ) ;
#4685 = EDGE_CURVE ( 'NONE', #1239, #4618, #2456, .T. ) ;
#4686 = AXIS2_PLACEMENT_3D ( 'NONE', #2050, #241, #1691 ) ;
#4687 = CARTESIAN_POINT ( 'NONE',  ( 3.993226401463535247, 31.01345121154055207, 9.266623410949817341 ) ) ;
#4688 = PRODUCT_CONTEXT ( 'NONE', #2446, 'mechanical' ) ;
#4689 = PLANE ( 'NONE',  #4661 ) ;
#4690 = FACE_OUTER_BOUND ( 'NONE', #2994, .T. ) ;
#4691 = DIRECTION ( 'NONE',  ( 0.000000000000000000, 0.000000000000000000, 1.000000000000000000 ) ) ;
#4692 =( GEOMETRIC_REPRESENTATION_CONTEXT ( 3 ) GLOBAL_UNCERTAINTY_ASSIGNED_CONTEXT ( ( #2662 ) ) GLOBAL_UNIT_ASSIGNED_CONTEXT ( ( #2852, #3187, #627 ) ) REPRESENTATION_CONTEXT ( 'NONE', 'WORKASPACE' ) );
#4693 = AXIS2_PLACEMENT_3D ( 'NONE', #2870, #3920, #4691 ) ;
#4694 = ORIENTED_EDGE ( 'NONE', *, *, #932, .F. ) ;
#4695 = ORIENTED_EDGE ( 'NONE', *, *, #3395, .F. ) ;
#4696 = STYLED_ITEM ( 'NONE', ( #929 ), #4382 ) ;
#4697 = CARTESIAN_POINT ( 'NONE',  ( 3.469446951953614189E-15, 40.00000000000000000, 3.999999999999990674 ) ) ;
#4698 = DIRECTION ( 'NONE',  ( 0.000000000000000000, 0.000000000000000000, 1.000000000000000000 ) ) ;
#4699 = CARTESIAN_POINT ( 'NONE',  ( 0.000000000000000000, 0.000000000000000000, 19.50000000000000000 ) ) ;
#4700 = ADVANCED_FACE ( 'NONE', ( #3881 ), #4650, .F. ) ;
#4701 = EDGE_LOOP ( 'NONE', ( #1293, #4559, #3470, #4451, #51, #188, #4055, #1774, #2894, #2950, #4419, #2827, #4091, #3660, #942, #1637, #3275, #4695, #2901 ) ) ;
#4702 = PLANE ( 'NONE',  #4666 ) ;
#4703 = FACE_OUTER_BOUND ( 'NONE', #1828, .T. ) ;
#4704 = FACE_OUTER_BOUND ( 'NONE', #2271, .T. ) ;
#4705 = CARTESIAN_POINT ( 'NONE',  ( 0.5208970779615244018, 29.99659053120184282, 12.97467366945674172 ) ) ;
#4706 = EDGE_CURVE ( 'NONE', #4498, #2297, #2415, .T. ) ;
#4707 = CARTESIAN_POINT ( 'NONE',  ( 24.00000000000000355, 0.000000000000000000, 19.00000000000000000 ) ) ;
#4708 = NEXT_ASSEMBLY_USAGE_OCCURRENCE ( 'NAUO1', ' ', ' ', #2248, #3648, $ ) ;
#4709 = NEXT_ASSEMBLY_USAGE_OCCURRENCE ( 'NAUO2', ' ', ' ', #2248, #3507, $ ) ;
#4710 = NEXT_ASSEMBLY_USAGE_OCCURRENCE ( 'NAUO3', ' ', ' ', #2248, #487, $ ) ;
#4711 = NEXT_ASSEMBLY_USAGE_OCCURRENCE ( 'NAUO4', ' ', ' ', #2248, #839, $ ) ;
#4712 = NEXT_ASSEMBLY_USAGE_OCCURRENCE ( 'NAUO5', ' ', ' ', #2248, #2893, $ ) ;
#4713 = NEXT_ASSEMBLY_USAGE_OCCURRENCE ( 'NAUO6', ' ', ' ', #2248, #1555, $ ) ;
#4714 = NEXT_ASSEMBLY_USAGE_OCCURRENCE ( 'NAUO7', ' ', ' ', #2248, #2956, $ ) ;
#4715 = NEXT_ASSEMBLY_USAGE_OCCURRENCE ( 'NAUO8', ' ', ' ', #2248, #1816, $ ) ;
#4716=COLOUR_RGB('Dark Blue',0.08,0.2,0.34);
#4717=FILL_AREA_STYLE_COLOUR('',#4716);
#4718=FILL_AREA_STYLE('',(#4717));
#4719=SURFACE_STYLE_FILL_AREA(#4718);
#4720=SURFACE_SIDE_STYLE('',(#4719));
#4721=SURFACE_STYLE_USAGE(.BOTH.,#4720);
#4722=PRESENTATION_STYLE_ASSIGNMENT((#4721));
#4723=COLOUR_RGB('Light Blue',0.38,0.62,0.78);
#4724=FILL_AREA_STYLE_COLOUR('',#4723);
#4725=FILL_AREA_STYLE('',(#4724));
#4726=SURFACE_STYLE_FILL_AREA(#4725);
#4727=SURFACE_SIDE_STYLE('',(#4726));
#4728=SURFACE_STYLE_USAGE(.BOTH.,#4727);
#4729=PRESENTATION_STYLE_ASSIGNMENT((#4728));
#4730=COLOUR_RGB('Sky Blue',0.24,0.69,0.87);
#4731=FILL_AREA_STYLE_COLOUR('',#4730);
#4732=FILL_AREA_STYLE('',(#4731));
#4733=SURFACE_STYLE_FILL_AREA(#4732);
#4734=SURFACE_SIDE_STYLE('',(#4733));
#4735=SURFACE_STYLE_USAGE(.BOTH.,#4734);
#4736=PRESENTATION_STYLE_ASSIGNMENT((#4735));
#4737=COLOUR_RGB('Grey',0.48,0.52,0.57);
#4738=FILL_AREA_STYLE_COLOUR('',#4737);
#4739=FILL_AREA_STYLE('',(#4738));
#4740=SURFACE_STYLE_FILL_AREA(#4739);
#4741=SURFACE_SIDE_STYLE('',(#4740));
#4742=SURFACE_STYLE_USAGE(.BOTH.,#4741);
#4743=PRESENTATION_STYLE_ASSIGNMENT((#4742));
#4744=COLOUR_RGB('Black',0.12,0.14,0.17);
#4745=FILL_AREA_STYLE_COLOUR('',#4744);
#4746=FILL_AREA_STYLE('',(#4745));
#4747=SURFACE_STYLE_FILL_AREA(#4746);
#4748=SURFACE_SIDE_STYLE('',(#4747));
#4749=SURFACE_STYLE_USAGE(.BOTH.,#4748);
#4750=PRESENTATION_STYLE_ASSIGNMENT((#4749));
#4751=COLOUR_RGB('Off White',0.89,0.88,0.83);
#4752=FILL_AREA_STYLE_COLOUR('',#4751);
#4753=FILL_AREA_STYLE('',(#4752));
#4754=SURFACE_STYLE_FILL_AREA(#4753);
#4755=SURFACE_SIDE_STYLE('',(#4754));
#4756=SURFACE_STYLE_USAGE(.BOTH.,#4755);
#4757=PRESENTATION_STYLE_ASSIGNMENT((#4756));
ENDSEC;
END-ISO-10303-21;
